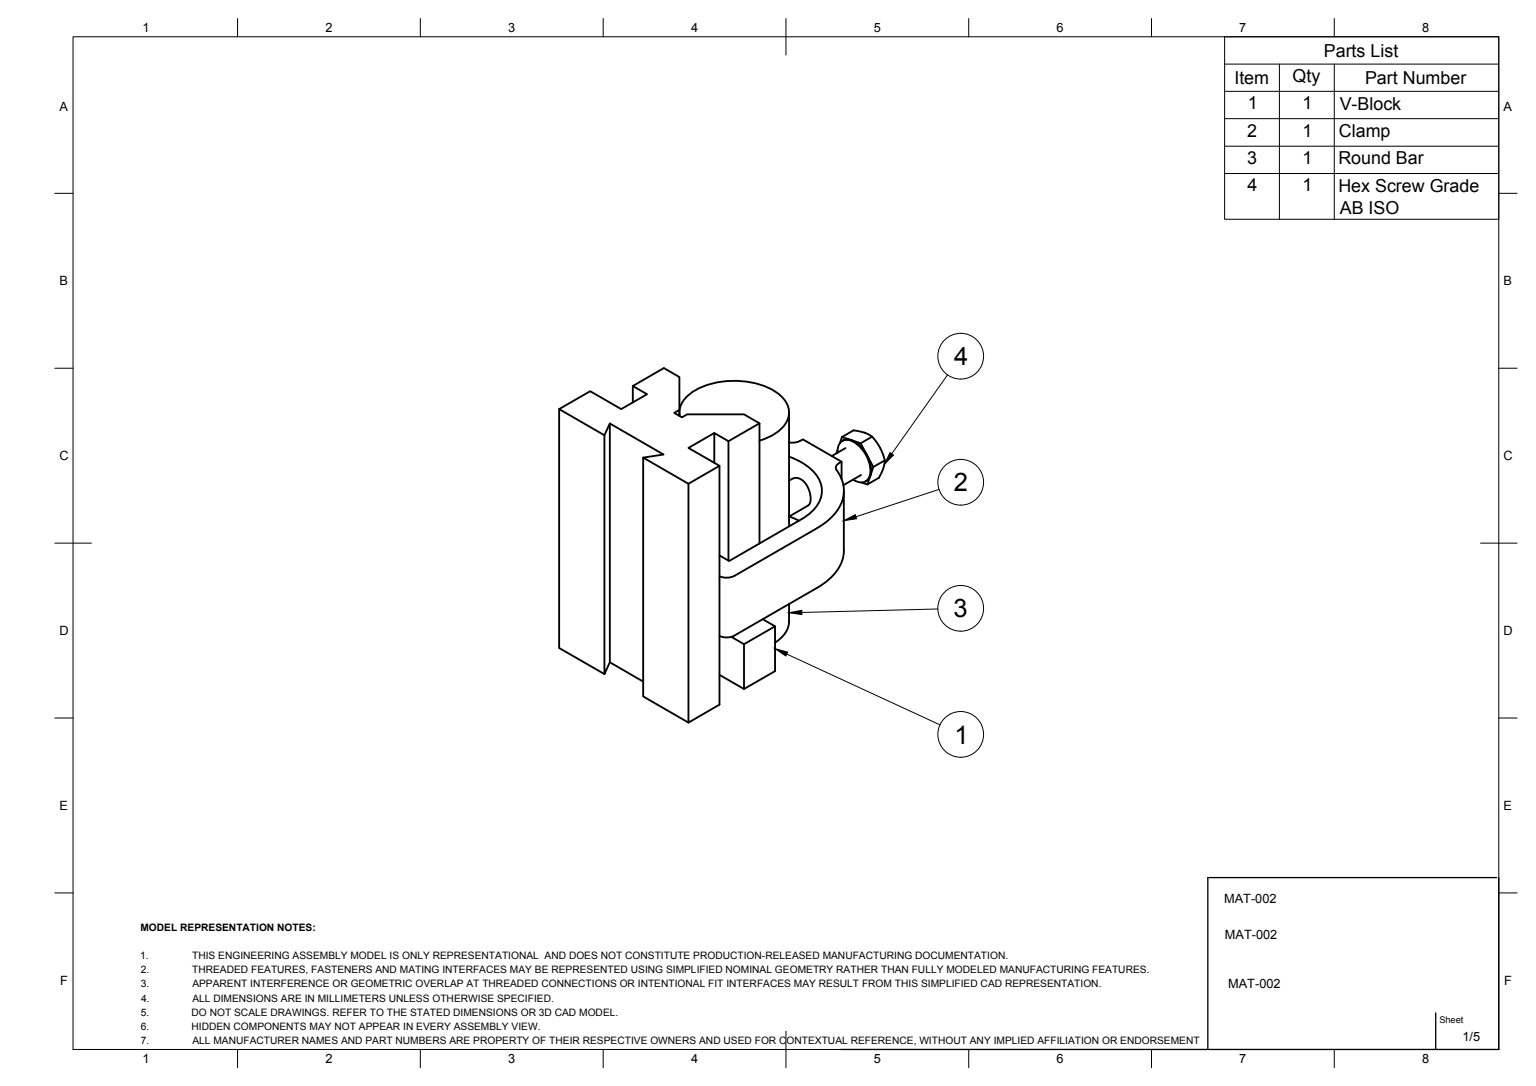
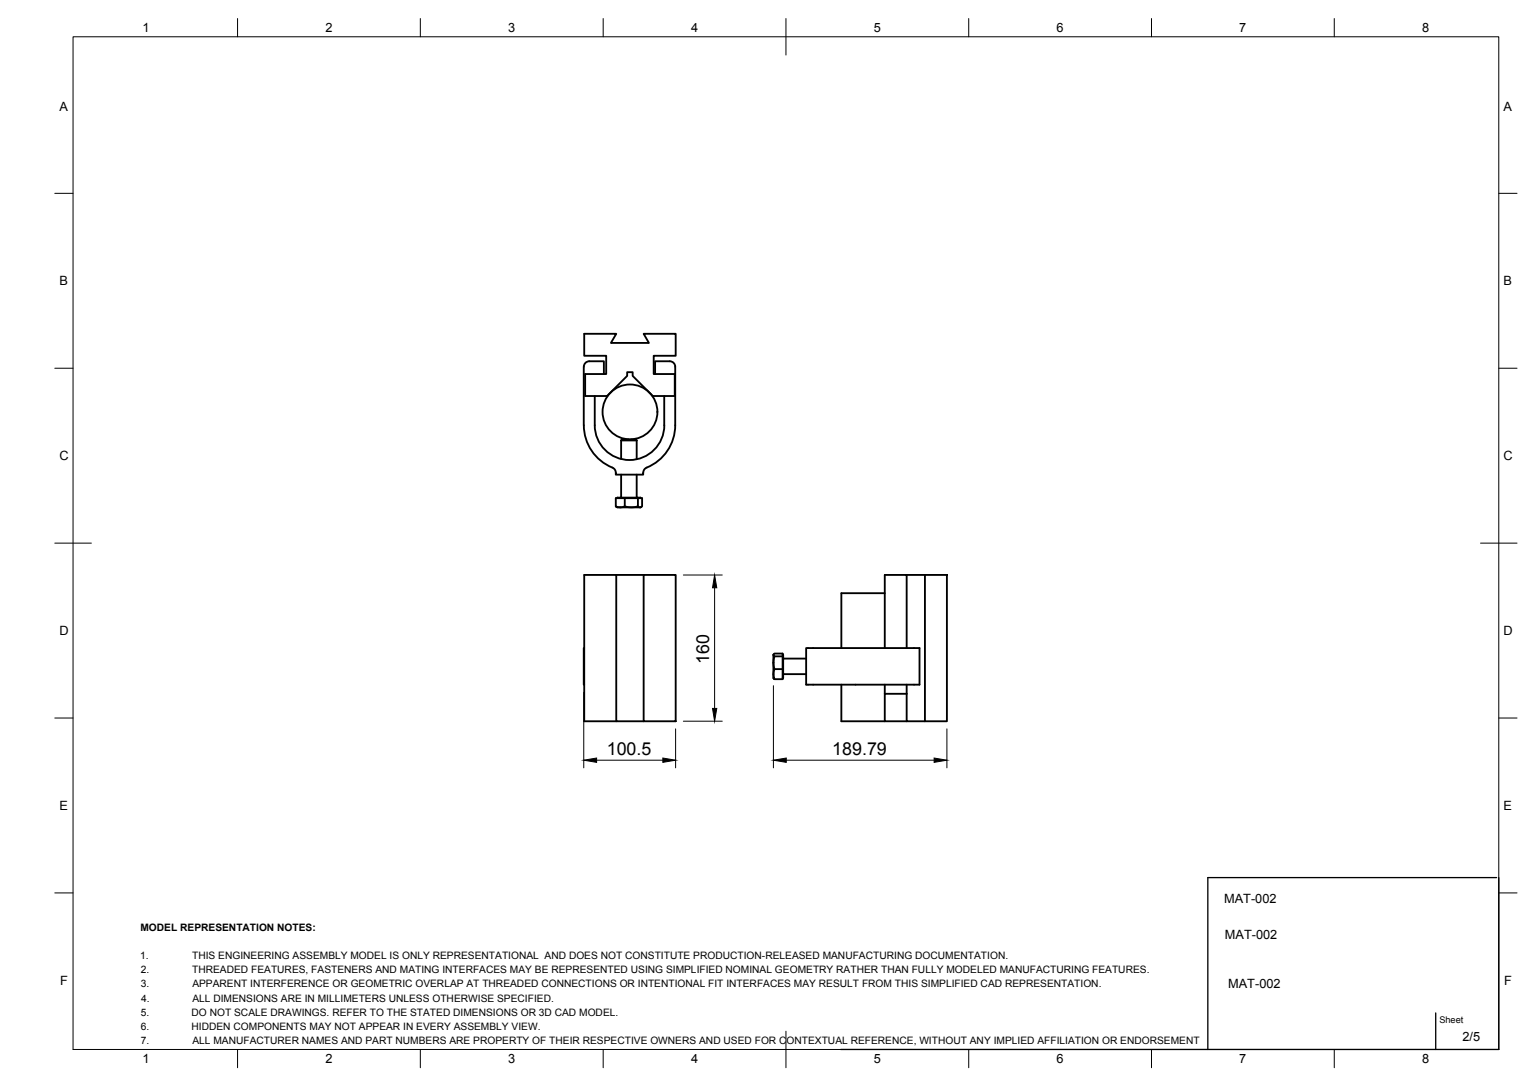
ISO-10303-21;
HEADER;
/* Generated by software containing ST-Developer
 * from STEP Tools, Inc. (www.steptools.com) 
 */

FILE_DESCRIPTION(
/* description */ ('STEP AP214'),
/* implementation_level */ '2;1');

FILE_NAME(
/* name */ 'MAT-002.step',
/* time_stamp */ '2026-11-14T04:35:10-08:00',
/* author */ (''),
/* organization */ (''),
/* preprocessor_version */ 'ST-DEVELOPER v20.2',
/* originating_system */ 'Autodesk Translation Framework v15.17.0.0',
/* authorisation */ '');

FILE_SCHEMA (('AUTOMOTIVE_DESIGN { 1 0 10303 214 3 1 1 }'));
ENDSEC;

DATA;
#10=MECHANICAL_DESIGN_GEOMETRIC_PRESENTATION_REPRESENTATION('',(#107,#108,
#109,#110),#2477);
#11=ITEM_DEFINED_TRANSFORMATION($,$,#1477,#1596);
#12=ITEM_DEFINED_TRANSFORMATION($,$,#1506,#1597);
#13=ITEM_DEFINED_TRANSFORMATION($,$,#1545,#1598);
#14=ITEM_DEFINED_TRANSFORMATION($,$,#1551,#1599);
#15=(
REPRESENTATION_RELATIONSHIP($,$,#2497,#2496)
REPRESENTATION_RELATIONSHIP_WITH_TRANSFORMATION(#11)
SHAPE_REPRESENTATION_RELATIONSHIP()
);
#16=(
REPRESENTATION_RELATIONSHIP($,$,#2498,#2496)
REPRESENTATION_RELATIONSHIP_WITH_TRANSFORMATION(#12)
SHAPE_REPRESENTATION_RELATIONSHIP()
);
#17=(
REPRESENTATION_RELATIONSHIP($,$,#2499,#2496)
REPRESENTATION_RELATIONSHIP_WITH_TRANSFORMATION(#13)
SHAPE_REPRESENTATION_RELATIONSHIP()
);
#18=(
REPRESENTATION_RELATIONSHIP($,$,#2500,#2496)
REPRESENTATION_RELATIONSHIP_WITH_TRANSFORMATION(#14)
SHAPE_REPRESENTATION_RELATIONSHIP()
);
#19=CONTEXT_DEPENDENT_SHAPE_REPRESENTATION(#15,#2492);
#20=CONTEXT_DEPENDENT_SHAPE_REPRESENTATION(#16,#2493);
#21=CONTEXT_DEPENDENT_SHAPE_REPRESENTATION(#17,#2494);
#22=CONTEXT_DEPENDENT_SHAPE_REPRESENTATION(#18,#2495);
#23=NEXT_ASSEMBLY_USAGE_OCCURRENCE('V-Block:1','V-Block:1','V-Block:1',
#2502,#2503,'V-Block:1');
#24=NEXT_ASSEMBLY_USAGE_OCCURRENCE('Clamp:1','Clamp:1','Clamp:1',#2502,
#2504,'Clamp:1');
#25=NEXT_ASSEMBLY_USAGE_OCCURRENCE('Round Bar:1','Round Bar:1',
'Round Bar:1',#2502,#2505,'Round Bar:1');
#26=NEXT_ASSEMBLY_USAGE_OCCURRENCE('Hex Screw Grade AB ISO:1',
'Hex Screw Grade AB ISO:1','Hex Screw Grade AB ISO:1',#2502,#2506,
'Hex Screw Grade AB ISO:1');
#27=(
BOUNDED_CURVE()
B_SPLINE_CURVE(2,(#2404,#2405,#2406),.UNSPECIFIED.,.F.,.F.)
B_SPLINE_CURVE_WITH_KNOTS((3,3),(-3.12660138416105,-1.84743207297635),
 .UNSPECIFIED.)
CURVE()
GEOMETRIC_REPRESENTATION_ITEM()
RATIONAL_B_SPLINE_CURVE((1.7511213796222,1.7511213796222,1.62539652116965))
REPRESENTATION_ITEM('')
);
#28=(
BOUNDED_CURVE()
B_SPLINE_CURVE(2,(#2407,#2408,#2409),.UNSPECIFIED.,.F.,.F.)
B_SPLINE_CURVE_WITH_KNOTS((3,3),(-4.40577069534575,-3.12660138416105),
 .UNSPECIFIED.)
CURVE()
GEOMETRIC_REPRESENTATION_ITEM()
RATIONAL_B_SPLINE_CURVE((1.62539652116964,1.75112137962219,1.75112137962219))
REPRESENTATION_ITEM('')
);
#29=(
BOUNDED_CURVE()
B_SPLINE_CURVE(2,(#2412,#2413,#2414),.UNSPECIFIED.,.F.,.F.)
B_SPLINE_CURVE_WITH_KNOTS((3,3),(-3.12660138416105,-1.84743207297636),
 .UNSPECIFIED.)
CURVE()
GEOMETRIC_REPRESENTATION_ITEM()
RATIONAL_B_SPLINE_CURVE((1.75112137962219,1.75112137962219,1.62539652116965))
REPRESENTATION_ITEM('')
);
#30=(
BOUNDED_CURVE()
B_SPLINE_CURVE(2,(#2415,#2416,#2417),.UNSPECIFIED.,.F.,.F.)
B_SPLINE_CURVE_WITH_KNOTS((3,3),(-4.40577069534575,-3.12660138416105),
 .UNSPECIFIED.)
CURVE()
GEOMETRIC_REPRESENTATION_ITEM()
RATIONAL_B_SPLINE_CURVE((1.62539652116965,1.7511213796222,1.7511213796222))
REPRESENTATION_ITEM('')
);
#31=(
BOUNDED_CURVE()
B_SPLINE_CURVE(2,(#2420,#2421,#2422),.UNSPECIFIED.,.F.,.F.)
B_SPLINE_CURVE_WITH_KNOTS((3,3),(-4.40577069534574,-3.12660138416105),
 .UNSPECIFIED.)
CURVE()
GEOMETRIC_REPRESENTATION_ITEM()
RATIONAL_B_SPLINE_CURVE((1.62539652116965,1.7511213796222,1.7511213796222))
REPRESENTATION_ITEM('')
);
#32=(
BOUNDED_CURVE()
B_SPLINE_CURVE(2,(#2423,#2424,#2425),.UNSPECIFIED.,.F.,.F.)
B_SPLINE_CURVE_WITH_KNOTS((3,3),(-3.12660138416105,-1.84743207297636),
 .UNSPECIFIED.)
CURVE()
GEOMETRIC_REPRESENTATION_ITEM()
RATIONAL_B_SPLINE_CURVE((1.75112137962219,1.75112137962219,1.62539652116965))
REPRESENTATION_ITEM('')
);
#33=(
BOUNDED_CURVE()
B_SPLINE_CURVE(2,(#2428,#2429,#2430),.UNSPECIFIED.,.F.,.F.)
B_SPLINE_CURVE_WITH_KNOTS((3,3),(-4.40577069534576,-3.12660138416105),
 .UNSPECIFIED.)
CURVE()
GEOMETRIC_REPRESENTATION_ITEM()
RATIONAL_B_SPLINE_CURVE((1.62539652116965,1.7511213796222,1.7511213796222))
REPRESENTATION_ITEM('')
);
#34=(
BOUNDED_CURVE()
B_SPLINE_CURVE(2,(#2431,#2432,#2433),.UNSPECIFIED.,.F.,.F.)
B_SPLINE_CURVE_WITH_KNOTS((3,3),(-3.12660138416105,-1.84743207297636),
 .UNSPECIFIED.)
CURVE()
GEOMETRIC_REPRESENTATION_ITEM()
RATIONAL_B_SPLINE_CURVE((1.75112137962219,1.75112137962219,1.62539652116965))
REPRESENTATION_ITEM('')
);
#35=(
BOUNDED_CURVE()
B_SPLINE_CURVE(2,(#2436,#2437,#2438),.UNSPECIFIED.,.F.,.F.)
B_SPLINE_CURVE_WITH_KNOTS((3,3),(-3.12660138416105,-1.84743207297636),
 .UNSPECIFIED.)
CURVE()
GEOMETRIC_REPRESENTATION_ITEM()
RATIONAL_B_SPLINE_CURVE((1.75112137962219,1.75112137962219,1.62539652116965))
REPRESENTATION_ITEM('')
);
#36=(
BOUNDED_CURVE()
B_SPLINE_CURVE(2,(#2439,#2440,#2441),.UNSPECIFIED.,.F.,.F.)
B_SPLINE_CURVE_WITH_KNOTS((3,3),(-4.40577069534574,-3.12660138416105),
 .UNSPECIFIED.)
CURVE()
GEOMETRIC_REPRESENTATION_ITEM()
RATIONAL_B_SPLINE_CURVE((1.62539652116965,1.75112137962219,1.75112137962219))
REPRESENTATION_ITEM('')
);
#37=(
BOUNDED_CURVE()
B_SPLINE_CURVE(2,(#2444,#2445,#2446),.UNSPECIFIED.,.F.,.F.)
B_SPLINE_CURVE_WITH_KNOTS((3,3),(-4.40577069534575,-3.12660138416105),
 .UNSPECIFIED.)
CURVE()
GEOMETRIC_REPRESENTATION_ITEM()
RATIONAL_B_SPLINE_CURVE((1.62539652116965,1.75112137962219,1.75112137962219))
REPRESENTATION_ITEM('')
);
#38=(
BOUNDED_CURVE()
B_SPLINE_CURVE(2,(#2447,#2448,#2449),.UNSPECIFIED.,.F.,.F.)
B_SPLINE_CURVE_WITH_KNOTS((3,3),(-3.12660138416105,-1.84743207297636),
 .UNSPECIFIED.)
CURVE()
GEOMETRIC_REPRESENTATION_ITEM()
RATIONAL_B_SPLINE_CURVE((1.75112137962219,1.75112137962219,1.62539652116964))
REPRESENTATION_ITEM('')
);
#39=CONICAL_SURFACE('',#1565,7.33266666666667,0.785398163397449);
#40=CONICAL_SURFACE('',#1584,12.75,1.0471975511966);
#41=CONICAL_SURFACE('',#1585,12.75,1.0471975511966);
#42=CONICAL_SURFACE('',#1586,12.75,1.0471975511966);
#43=CONICAL_SURFACE('',#1587,12.75,1.0471975511966);
#44=CONICAL_SURFACE('',#1588,12.75,1.0471975511966);
#45=CONICAL_SURFACE('',#1589,12.75,1.0471975511966);
#46=TOROIDAL_SURFACE('',#1552,9.06666666666667,0.566666666666667);
#47=FACE_BOUND('',#226,.T.);
#48=FACE_BOUND('',#235,.T.);
#49=FACE_BOUND('',#255,.T.);
#50=CIRCLE('',#1508,8.49999999999998);
#51=CIRCLE('',#1512,38.);
#52=CIRCLE('',#1513,38.);
#53=CIRCLE('',#1520,50.);
#54=CIRCLE('',#1521,50.);
#55=CIRCLE('',#1526,50.);
#56=CIRCLE('',#1527,50.);
#57=CIRCLE('',#1532,6.);
#58=CIRCLE('',#1533,6.);
#59=CIRCLE('',#1534,6.);
#60=CIRCLE('',#1535,6.);
#61=CIRCLE('',#1537,6.);
#62=CIRCLE('',#1538,6.);
#63=CIRCLE('',#1539,6.);
#64=CIRCLE('',#1540,6.);
#65=CIRCLE('',#1547,30.);
#66=CIRCLE('',#1548,30.);
#67=CIRCLE('',#1553,8.5);
#68=CIRCLE('',#1554,8.5);
#69=CIRCLE('',#1555,0.566666666666667);
#70=CIRCLE('',#1556,9.06666666666667);
#71=CIRCLE('',#1558,12.75);
#72=CIRCLE('',#1559,12.75);
#73=CIRCLE('',#1560,12.75);
#74=CIRCLE('',#1561,12.75);
#75=CIRCLE('',#1562,12.75);
#76=CIRCLE('',#1563,12.75);
#77=CIRCLE('',#1564,12.75);
#78=CIRCLE('',#1566,8.5);
#79=CIRCLE('',#1567,7.33266666666667);
#80=CIRCLE('',#1578,12.75);
#81=CIRCLE('',#1579,12.75);
#82=CIRCLE('',#1580,12.75);
#83=CIRCLE('',#1581,12.75);
#84=CIRCLE('',#1582,12.75);
#85=CIRCLE('',#1583,12.75);
#86=B_SPLINE_CURVE_WITH_KNOTS('',3,(#2159,#2160,#2161,#2162,#2163,#2164,
#2165,#2166,#2167,#2168,#2169,#2170,#2171,#2172,#2173,#2174,#2175,#2176,
#2177),.UNSPECIFIED.,.F.,.F.,(4,2,2,2,3,2,2,2,4),(3.85552474626411,4.17737028900463,
4.49921583174514,4.82064221776852,5.14206860379189,5.46349498981527,5.78492137583865,
6.10676691857916,6.42861246131968),.UNSPECIFIED.);
#87=B_SPLINE_CURVE_WITH_KNOTS('',3,(#2181,#2182,#2183,#2184,#2185,#2186,
#2187,#2188,#2189,#2190,#2191,#2192,#2193,#2194,#2195,#2196,#2197,#2198),
 .UNSPECIFIED.,.F.,.F.,(4,2,2,2,2,2,2,2,4),(6.42861246131968,6.74954370836776,
7.07047495541584,7.39178893055184,7.71310290568784,8.03441688082384,8.35573085595985,
8.67666210300793,8.99759335005601),.UNSPECIFIED.);
#88=CYLINDRICAL_SURFACE('',#1507,8.49999999999998);
#89=CYLINDRICAL_SURFACE('',#1511,38.);
#90=CYLINDRICAL_SURFACE('',#1519,50.);
#91=CYLINDRICAL_SURFACE('',#1525,50.);
#92=CYLINDRICAL_SURFACE('',#1541,6.);
#93=CYLINDRICAL_SURFACE('',#1542,6.);
#94=CYLINDRICAL_SURFACE('',#1543,6.);
#95=CYLINDRICAL_SURFACE('',#1544,6.);
#96=CYLINDRICAL_SURFACE('',#1546,30.);
#97=CYLINDRICAL_SURFACE('',#1557,12.75);
#98=CYLINDRICAL_SURFACE('',#1568,8.5);
#99=SHAPE_REPRESENTATION_RELATIONSHIP('SRR','None',#2497,#103);
#100=SHAPE_REPRESENTATION_RELATIONSHIP('SRR','None',#2498,#104);
#101=SHAPE_REPRESENTATION_RELATIONSHIP('SRR','None',#2499,#105);
#102=SHAPE_REPRESENTATION_RELATIONSHIP('SRR','None',#2500,#106);
#103=ADVANCED_BREP_SHAPE_REPRESENTATION('',(#111),#2473);
#104=ADVANCED_BREP_SHAPE_REPRESENTATION('',(#112),#2474);
#105=ADVANCED_BREP_SHAPE_REPRESENTATION('',(#113),#2475);
#106=ADVANCED_BREP_SHAPE_REPRESENTATION('',(#114),#2476);
#107=STYLED_ITEM('',(#2526),#111);
#108=STYLED_ITEM('',(#2527),#112);
#109=STYLED_ITEM('',(#2528),#113);
#110=STYLED_ITEM('',(#2529),#114);
#111=MANIFOLD_SOLID_BREP('Body1',#1427);
#112=MANIFOLD_SOLID_BREP('Body1',#1428);
#113=MANIFOLD_SOLID_BREP('Body1',#1429);
#114=MANIFOLD_SOLID_BREP('Body1',#1430);
#115=FACE_OUTER_BOUND('',#194,.T.);
#116=FACE_OUTER_BOUND('',#195,.T.);
#117=FACE_OUTER_BOUND('',#196,.T.);
#118=FACE_OUTER_BOUND('',#197,.T.);
#119=FACE_OUTER_BOUND('',#198,.T.);
#120=FACE_OUTER_BOUND('',#199,.T.);
#121=FACE_OUTER_BOUND('',#200,.T.);
#122=FACE_OUTER_BOUND('',#201,.T.);
#123=FACE_OUTER_BOUND('',#202,.T.);
#124=FACE_OUTER_BOUND('',#203,.T.);
#125=FACE_OUTER_BOUND('',#204,.T.);
#126=FACE_OUTER_BOUND('',#205,.T.);
#127=FACE_OUTER_BOUND('',#206,.T.);
#128=FACE_OUTER_BOUND('',#207,.T.);
#129=FACE_OUTER_BOUND('',#208,.T.);
#130=FACE_OUTER_BOUND('',#209,.T.);
#131=FACE_OUTER_BOUND('',#210,.T.);
#132=FACE_OUTER_BOUND('',#211,.T.);
#133=FACE_OUTER_BOUND('',#212,.T.);
#134=FACE_OUTER_BOUND('',#213,.T.);
#135=FACE_OUTER_BOUND('',#214,.T.);
#136=FACE_OUTER_BOUND('',#215,.T.);
#137=FACE_OUTER_BOUND('',#216,.T.);
#138=FACE_OUTER_BOUND('',#217,.T.);
#139=FACE_OUTER_BOUND('',#218,.T.);
#140=FACE_OUTER_BOUND('',#219,.T.);
#141=FACE_OUTER_BOUND('',#220,.T.);
#142=FACE_OUTER_BOUND('',#221,.T.);
#143=FACE_OUTER_BOUND('',#222,.T.);
#144=FACE_OUTER_BOUND('',#223,.T.);
#145=FACE_OUTER_BOUND('',#224,.T.);
#146=FACE_OUTER_BOUND('',#225,.T.);
#147=FACE_OUTER_BOUND('',#227,.T.);
#148=FACE_OUTER_BOUND('',#228,.T.);
#149=FACE_OUTER_BOUND('',#229,.T.);
#150=FACE_OUTER_BOUND('',#230,.T.);
#151=FACE_OUTER_BOUND('',#231,.T.);
#152=FACE_OUTER_BOUND('',#232,.T.);
#153=FACE_OUTER_BOUND('',#233,.T.);
#154=FACE_OUTER_BOUND('',#234,.T.);
#155=FACE_OUTER_BOUND('',#236,.T.);
#156=FACE_OUTER_BOUND('',#237,.T.);
#157=FACE_OUTER_BOUND('',#238,.T.);
#158=FACE_OUTER_BOUND('',#239,.T.);
#159=FACE_OUTER_BOUND('',#240,.T.);
#160=FACE_OUTER_BOUND('',#241,.T.);
#161=FACE_OUTER_BOUND('',#242,.T.);
#162=FACE_OUTER_BOUND('',#243,.T.);
#163=FACE_OUTER_BOUND('',#244,.T.);
#164=FACE_OUTER_BOUND('',#245,.T.);
#165=FACE_OUTER_BOUND('',#246,.T.);
#166=FACE_OUTER_BOUND('',#247,.T.);
#167=FACE_OUTER_BOUND('',#248,.T.);
#168=FACE_OUTER_BOUND('',#249,.T.);
#169=FACE_OUTER_BOUND('',#250,.T.);
#170=FACE_OUTER_BOUND('',#251,.T.);
#171=FACE_OUTER_BOUND('',#252,.T.);
#172=FACE_OUTER_BOUND('',#253,.T.);
#173=FACE_OUTER_BOUND('',#254,.T.);
#174=FACE_OUTER_BOUND('',#256,.T.);
#175=FACE_OUTER_BOUND('',#257,.T.);
#176=FACE_OUTER_BOUND('',#258,.T.);
#177=FACE_OUTER_BOUND('',#259,.T.);
#178=FACE_OUTER_BOUND('',#260,.T.);
#179=FACE_OUTER_BOUND('',#261,.T.);
#180=FACE_OUTER_BOUND('',#262,.T.);
#181=FACE_OUTER_BOUND('',#263,.T.);
#182=FACE_OUTER_BOUND('',#264,.T.);
#183=FACE_OUTER_BOUND('',#265,.T.);
#184=FACE_OUTER_BOUND('',#266,.T.);
#185=FACE_OUTER_BOUND('',#267,.T.);
#186=FACE_OUTER_BOUND('',#268,.T.);
#187=FACE_OUTER_BOUND('',#269,.T.);
#188=FACE_OUTER_BOUND('',#270,.T.);
#189=FACE_OUTER_BOUND('',#271,.T.);
#190=FACE_OUTER_BOUND('',#272,.T.);
#191=FACE_OUTER_BOUND('',#273,.T.);
#192=FACE_OUTER_BOUND('',#274,.T.);
#193=FACE_OUTER_BOUND('',#275,.T.);
#194=EDGE_LOOP('',(#894,#895,#896,#897));
#195=EDGE_LOOP('',(#898,#899,#900,#901));
#196=EDGE_LOOP('',(#902,#903,#904,#905));
#197=EDGE_LOOP('',(#906,#907,#908,#909));
#198=EDGE_LOOP('',(#910,#911,#912,#913));
#199=EDGE_LOOP('',(#914,#915,#916,#917,#918,#919));
#200=EDGE_LOOP('',(#920,#921,#922,#923,#924,#925));
#201=EDGE_LOOP('',(#926,#927,#928,#929));
#202=EDGE_LOOP('',(#930,#931,#932,#933));
#203=EDGE_LOOP('',(#934,#935,#936,#937));
#204=EDGE_LOOP('',(#938,#939,#940,#941));
#205=EDGE_LOOP('',(#942,#943,#944,#945));
#206=EDGE_LOOP('',(#946,#947,#948,#949,#950,#951));
#207=EDGE_LOOP('',(#952,#953,#954,#955,#956,#957));
#208=EDGE_LOOP('',(#958,#959,#960,#961));
#209=EDGE_LOOP('',(#962,#963,#964,#965));
#210=EDGE_LOOP('',(#966,#967,#968,#969));
#211=EDGE_LOOP('',(#970,#971,#972,#973));
#212=EDGE_LOOP('',(#974,#975,#976,#977));
#213=EDGE_LOOP('',(#978,#979,#980,#981));
#214=EDGE_LOOP('',(#982,#983,#984,#985));
#215=EDGE_LOOP('',(#986,#987,#988,#989));
#216=EDGE_LOOP('',(#990,#991,#992,#993,#994,#995,#996,#997,#998,#999,#1000,
#1001,#1002,#1003,#1004,#1005,#1006,#1007,#1008,#1009,#1010,#1011));
#217=EDGE_LOOP('',(#1012,#1013,#1014,#1015,#1016,#1017,#1018,#1019,#1020,
#1021,#1022,#1023,#1024,#1025,#1026,#1027,#1028,#1029,#1030,#1031,#1032,
#1033));
#218=EDGE_LOOP('',(#1034,#1035,#1036,#1037));
#219=EDGE_LOOP('',(#1038,#1039,#1040,#1041));
#220=EDGE_LOOP('',(#1042,#1043,#1044,#1045));
#221=EDGE_LOOP('',(#1046,#1047,#1048,#1049));
#222=EDGE_LOOP('',(#1050,#1051,#1052,#1053,#1054));
#223=EDGE_LOOP('',(#1055,#1056,#1057,#1058));
#224=EDGE_LOOP('',(#1059,#1060,#1061,#1062));
#225=EDGE_LOOP('',(#1063,#1064,#1065,#1066));
#226=EDGE_LOOP('',(#1067,#1068));
#227=EDGE_LOOP('',(#1069,#1070,#1071,#1072));
#228=EDGE_LOOP('',(#1073,#1074,#1075,#1076));
#229=EDGE_LOOP('',(#1077,#1078,#1079,#1080));
#230=EDGE_LOOP('',(#1081,#1082,#1083,#1084));
#231=EDGE_LOOP('',(#1085,#1086,#1087,#1088));
#232=EDGE_LOOP('',(#1089,#1090,#1091,#1092));
#233=EDGE_LOOP('',(#1093,#1094,#1095,#1096));
#234=EDGE_LOOP('',(#1097,#1098,#1099,#1100));
#235=EDGE_LOOP('',(#1101));
#236=EDGE_LOOP('',(#1102,#1103,#1104,#1105));
#237=EDGE_LOOP('',(#1106,#1107,#1108,#1109));
#238=EDGE_LOOP('',(#1110,#1111,#1112,#1113));
#239=EDGE_LOOP('',(#1114,#1115,#1116,#1117));
#240=EDGE_LOOP('',(#1118,#1119,#1120,#1121));
#241=EDGE_LOOP('',(#1122,#1123,#1124,#1125,#1126,#1127,#1128,#1129,#1130,
#1131,#1132,#1133,#1134,#1135,#1136,#1137,#1138,#1139,#1140,#1141));
#242=EDGE_LOOP('',(#1142,#1143,#1144,#1145,#1146,#1147,#1148,#1149,#1150,
#1151,#1152,#1153,#1154,#1155,#1156,#1157,#1158,#1159,#1160,#1161));
#243=EDGE_LOOP('',(#1162,#1163,#1164,#1165));
#244=EDGE_LOOP('',(#1166,#1167,#1168,#1169));
#245=EDGE_LOOP('',(#1170,#1171,#1172,#1173));
#246=EDGE_LOOP('',(#1174,#1175,#1176,#1177));
#247=EDGE_LOOP('',(#1178,#1179,#1180,#1181));
#248=EDGE_LOOP('',(#1182));
#249=EDGE_LOOP('',(#1183));
#250=EDGE_LOOP('',(#1184,#1185,#1186,#1187,#1188));
#251=EDGE_LOOP('',(#1189,#1190,#1191,#1192,#1193,#1194,#1195,#1196,#1197));
#252=EDGE_LOOP('',(#1198,#1199,#1200,#1201));
#253=EDGE_LOOP('',(#1202,#1203,#1204,#1205,#1206));
#254=EDGE_LOOP('',(#1207));
#255=EDGE_LOOP('',(#1208));
#256=EDGE_LOOP('',(#1209));
#257=EDGE_LOOP('',(#1210,#1211,#1212));
#258=EDGE_LOOP('',(#1213,#1214,#1215));
#259=EDGE_LOOP('',(#1216,#1217,#1218));
#260=EDGE_LOOP('',(#1219,#1220,#1221));
#261=EDGE_LOOP('',(#1222,#1223,#1224));
#262=EDGE_LOOP('',(#1225,#1226,#1227));
#263=EDGE_LOOP('',(#1228,#1229,#1230,#1231,#1232,#1233));
#264=EDGE_LOOP('',(#1234,#1235,#1236));
#265=EDGE_LOOP('',(#1237,#1238,#1239));
#266=EDGE_LOOP('',(#1240,#1241,#1242));
#267=EDGE_LOOP('',(#1243,#1244,#1245));
#268=EDGE_LOOP('',(#1246,#1247,#1248));
#269=EDGE_LOOP('',(#1249,#1250,#1251));
#270=EDGE_LOOP('',(#1252,#1253,#1254,#1255,#1256,#1257));
#271=EDGE_LOOP('',(#1258,#1259,#1260,#1261,#1262,#1263));
#272=EDGE_LOOP('',(#1264,#1265,#1266,#1267,#1268,#1269));
#273=EDGE_LOOP('',(#1270,#1271,#1272,#1273,#1274,#1275));
#274=EDGE_LOOP('',(#1276,#1277,#1278,#1279,#1280,#1281));
#275=EDGE_LOOP('',(#1282,#1283,#1284,#1285,#1286,#1287));
#276=LINE('',#2000,#423);
#277=LINE('',#2002,#424);
#278=LINE('',#2004,#425);
#279=LINE('',#2005,#426);
#280=LINE('',#2009,#427);
#281=LINE('',#2011,#428);
#282=LINE('',#2013,#429);
#283=LINE('',#2014,#430);
#284=LINE('',#2018,#431);
#285=LINE('',#2020,#432);
#286=LINE('',#2022,#433);
#287=LINE('',#2023,#434);
#288=LINE('',#2026,#435);
#289=LINE('',#2028,#436);
#290=LINE('',#2029,#437);
#291=LINE('',#2032,#438);
#292=LINE('',#2034,#439);
#293=LINE('',#2035,#440);
#294=LINE('',#2037,#441);
#295=LINE('',#2039,#442);
#296=LINE('',#2041,#443);
#297=LINE('',#2042,#444);
#298=LINE('',#2045,#445);
#299=LINE('',#2047,#446);
#300=LINE('',#2049,#447);
#301=LINE('',#2051,#448);
#302=LINE('',#2052,#449);
#303=LINE('',#2055,#450);
#304=LINE('',#2057,#451);
#305=LINE('',#2058,#452);
#306=LINE('',#2061,#453);
#307=LINE('',#2063,#454);
#308=LINE('',#2064,#455);
#309=LINE('',#2067,#456);
#310=LINE('',#2069,#457);
#311=LINE('',#2070,#458);
#312=LINE('',#2073,#459);
#313=LINE('',#2075,#460);
#314=LINE('',#2076,#461);
#315=LINE('',#2079,#462);
#316=LINE('',#2081,#463);
#317=LINE('',#2082,#464);
#318=LINE('',#2084,#465);
#319=LINE('',#2086,#466);
#320=LINE('',#2088,#467);
#321=LINE('',#2089,#468);
#322=LINE('',#2092,#469);
#323=LINE('',#2094,#470);
#324=LINE('',#2096,#471);
#325=LINE('',#2098,#472);
#326=LINE('',#2099,#473);
#327=LINE('',#2102,#474);
#328=LINE('',#2104,#475);
#329=LINE('',#2105,#476);
#330=LINE('',#2108,#477);
#331=LINE('',#2110,#478);
#332=LINE('',#2111,#479);
#333=LINE('',#2114,#480);
#334=LINE('',#2116,#481);
#335=LINE('',#2117,#482);
#336=LINE('',#2120,#483);
#337=LINE('',#2122,#484);
#338=LINE('',#2123,#485);
#339=LINE('',#2126,#486);
#340=LINE('',#2128,#487);
#341=LINE('',#2129,#488);
#342=LINE('',#2132,#489);
#343=LINE('',#2134,#490);
#344=LINE('',#2135,#491);
#345=LINE('',#2138,#492);
#346=LINE('',#2140,#493);
#347=LINE('',#2141,#494);
#348=LINE('',#2143,#495);
#349=LINE('',#2144,#496);
#350=LINE('',#2146,#497);
#351=LINE('',#2147,#498);
#352=LINE('',#2150,#499);
#353=LINE('',#2153,#500);
#354=LINE('',#2179,#501);
#355=LINE('',#2202,#502);
#356=LINE('',#2204,#503);
#357=LINE('',#2206,#504);
#358=LINE('',#2207,#505);
#359=LINE('',#2210,#506);
#360=LINE('',#2212,#507);
#361=LINE('',#2213,#508);
#362=LINE('',#2218,#509);
#363=LINE('',#2222,#510);
#364=LINE('',#2224,#511);
#365=LINE('',#2225,#512);
#366=LINE('',#2228,#513);
#367=LINE('',#2230,#514);
#368=LINE('',#2231,#515);
#369=LINE('',#2234,#516);
#370=LINE('',#2236,#517);
#371=LINE('',#2237,#518);
#372=LINE('',#2240,#519);
#373=LINE('',#2242,#520);
#374=LINE('',#2243,#521);
#375=LINE('',#2247,#522);
#376=LINE('',#2249,#523);
#377=LINE('',#2251,#524);
#378=LINE('',#2252,#525);
#379=LINE('',#2257,#526);
#380=LINE('',#2262,#527);
#381=LINE('',#2264,#528);
#382=LINE('',#2266,#529);
#383=LINE('',#2267,#530);
#384=LINE('',#2270,#531);
#385=LINE('',#2272,#532);
#386=LINE('',#2273,#533);
#387=LINE('',#2276,#534);
#388=LINE('',#2278,#535);
#389=LINE('',#2279,#536);
#390=LINE('',#2285,#537);
#391=LINE('',#2288,#538);
#392=LINE('',#2291,#539);
#393=LINE('',#2293,#540);
#394=LINE('',#2294,#541);
#395=LINE('',#2298,#542);
#396=LINE('',#2300,#543);
#397=LINE('',#2302,#544);
#398=LINE('',#2303,#545);
#399=LINE('',#2305,#546);
#400=LINE('',#2306,#547);
#401=LINE('',#2326,#548);
#402=LINE('',#2348,#549);
#403=LINE('',#2359,#550);
#404=LINE('',#2362,#551);
#405=LINE('',#2367,#552);
#406=LINE('',#2368,#553);
#407=LINE('',#2371,#554);
#408=LINE('',#2372,#555);
#409=LINE('',#2375,#556);
#410=LINE('',#2376,#557);
#411=LINE('',#2379,#558);
#412=LINE('',#2380,#559);
#413=LINE('',#2383,#560);
#414=LINE('',#2384,#561);
#415=LINE('',#2387,#562);
#416=LINE('',#2388,#563);
#417=LINE('',#2451,#564);
#418=LINE('',#2452,#565);
#419=LINE('',#2454,#566);
#420=LINE('',#2456,#567);
#421=LINE('',#2458,#568);
#422=LINE('',#2460,#569);
#423=VECTOR('',#1606,1000.);
#424=VECTOR('',#1607,1000.);
#425=VECTOR('',#1608,1000.);
#426=VECTOR('',#1609,1000.);
#427=VECTOR('',#1612,1000.);
#428=VECTOR('',#1613,1000.);
#429=VECTOR('',#1614,1000.);
#430=VECTOR('',#1615,1000.);
#431=VECTOR('',#1618,1000.);
#432=VECTOR('',#1619,1000.);
#433=VECTOR('',#1620,1000.);
#434=VECTOR('',#1621,1000.);
#435=VECTOR('',#1624,1000.);
#436=VECTOR('',#1625,1000.);
#437=VECTOR('',#1626,1000.);
#438=VECTOR('',#1629,1000.);
#439=VECTOR('',#1630,1000.);
#440=VECTOR('',#1631,1000.);
#441=VECTOR('',#1634,1000.);
#442=VECTOR('',#1635,1000.);
#443=VECTOR('',#1636,1000.);
#444=VECTOR('',#1637,1000.);
#445=VECTOR('',#1640,1000.);
#446=VECTOR('',#1641,1000.);
#447=VECTOR('',#1642,1000.);
#448=VECTOR('',#1643,1000.);
#449=VECTOR('',#1644,1000.);
#450=VECTOR('',#1647,1000.);
#451=VECTOR('',#1648,1000.);
#452=VECTOR('',#1649,1000.);
#453=VECTOR('',#1652,1000.);
#454=VECTOR('',#1653,1000.);
#455=VECTOR('',#1654,1000.);
#456=VECTOR('',#1657,1000.);
#457=VECTOR('',#1658,1000.);
#458=VECTOR('',#1659,1000.);
#459=VECTOR('',#1662,1000.);
#460=VECTOR('',#1663,1000.);
#461=VECTOR('',#1664,1000.);
#462=VECTOR('',#1667,1000.);
#463=VECTOR('',#1668,1000.);
#464=VECTOR('',#1669,1000.);
#465=VECTOR('',#1672,1000.);
#466=VECTOR('',#1673,1000.);
#467=VECTOR('',#1674,1000.);
#468=VECTOR('',#1675,1000.);
#469=VECTOR('',#1678,1000.);
#470=VECTOR('',#1679,1000.);
#471=VECTOR('',#1680,1000.);
#472=VECTOR('',#1681,1000.);
#473=VECTOR('',#1682,1000.);
#474=VECTOR('',#1685,1000.);
#475=VECTOR('',#1686,1000.);
#476=VECTOR('',#1687,1000.);
#477=VECTOR('',#1690,1000.);
#478=VECTOR('',#1691,1000.);
#479=VECTOR('',#1692,1000.);
#480=VECTOR('',#1695,1000.);
#481=VECTOR('',#1696,1000.);
#482=VECTOR('',#1697,1000.);
#483=VECTOR('',#1700,1000.);
#484=VECTOR('',#1701,1000.);
#485=VECTOR('',#1702,1000.);
#486=VECTOR('',#1705,1000.);
#487=VECTOR('',#1706,1000.);
#488=VECTOR('',#1707,1000.);
#489=VECTOR('',#1710,1000.);
#490=VECTOR('',#1711,1000.);
#491=VECTOR('',#1712,1000.);
#492=VECTOR('',#1715,1000.);
#493=VECTOR('',#1716,1000.);
#494=VECTOR('',#1717,1000.);
#495=VECTOR('',#1720,1000.);
#496=VECTOR('',#1721,1000.);
#497=VECTOR('',#1724,1000.);
#498=VECTOR('',#1725,1000.);
#499=VECTOR('',#1730,1000.);
#500=VECTOR('',#1735,1000.);
#501=VECTOR('',#1742,8.49999999999998);
#502=VECTOR('',#1747,1000.);
#503=VECTOR('',#1748,1000.);
#504=VECTOR('',#1749,1000.);
#505=VECTOR('',#1750,1000.);
#506=VECTOR('',#1753,1000.);
#507=VECTOR('',#1754,1000.);
#508=VECTOR('',#1755,1000.);
#509=VECTOR('',#1760,1000.);
#510=VECTOR('',#1765,1000.);
#511=VECTOR('',#1766,1000.);
#512=VECTOR('',#1767,1000.);
#513=VECTOR('',#1770,1000.);
#514=VECTOR('',#1771,1000.);
#515=VECTOR('',#1772,1000.);
#516=VECTOR('',#1775,1000.);
#517=VECTOR('',#1776,1000.);
#518=VECTOR('',#1777,1000.);
#519=VECTOR('',#1780,1000.);
#520=VECTOR('',#1781,1000.);
#521=VECTOR('',#1782,1000.);
#522=VECTOR('',#1785,1000.);
#523=VECTOR('',#1786,1000.);
#524=VECTOR('',#1787,1000.);
#525=VECTOR('',#1788,1000.);
#526=VECTOR('',#1793,1000.);
#527=VECTOR('',#1798,1000.);
#528=VECTOR('',#1799,1000.);
#529=VECTOR('',#1800,1000.);
#530=VECTOR('',#1801,1000.);
#531=VECTOR('',#1804,1000.);
#532=VECTOR('',#1805,1000.);
#533=VECTOR('',#1806,1000.);
#534=VECTOR('',#1809,1000.);
#535=VECTOR('',#1810,1000.);
#536=VECTOR('',#1811,1000.);
#537=VECTOR('',#1816,1000.);
#538=VECTOR('',#1819,1000.);
#539=VECTOR('',#1822,1000.);
#540=VECTOR('',#1823,1000.);
#541=VECTOR('',#1824,1000.);
#542=VECTOR('',#1827,1000.);
#543=VECTOR('',#1828,1000.);
#544=VECTOR('',#1829,1000.);
#545=VECTOR('',#1830,1000.);
#546=VECTOR('',#1833,1000.);
#547=VECTOR('',#1834,1000.);
#548=VECTOR('',#1869,30.);
#549=VECTOR('',#1896,12.75);
#550=VECTOR('',#1909,7.33266666666667);
#551=VECTOR('',#1914,8.5);
#552=VECTOR('',#1921,1000.);
#553=VECTOR('',#1922,1000.);
#554=VECTOR('',#1925,1000.);
#555=VECTOR('',#1926,1000.);
#556=VECTOR('',#1929,1000.);
#557=VECTOR('',#1930,1000.);
#558=VECTOR('',#1933,1000.);
#559=VECTOR('',#1934,1000.);
#560=VECTOR('',#1937,1000.);
#561=VECTOR('',#1938,1000.);
#562=VECTOR('',#1941,1000.);
#563=VECTOR('',#1942,1000.);
#564=VECTOR('',#1971,1000.);
#565=VECTOR('',#1972,1000.);
#566=VECTOR('',#1975,1000.);
#567=VECTOR('',#1978,1000.);
#568=VECTOR('',#1981,1000.);
#569=VECTOR('',#1984,1000.);
#570=VERTEX_POINT('',#1998);
#571=VERTEX_POINT('',#1999);
#572=VERTEX_POINT('',#2001);
#573=VERTEX_POINT('',#2003);
#574=VERTEX_POINT('',#2007);
#575=VERTEX_POINT('',#2008);
#576=VERTEX_POINT('',#2010);
#577=VERTEX_POINT('',#2012);
#578=VERTEX_POINT('',#2016);
#579=VERTEX_POINT('',#2017);
#580=VERTEX_POINT('',#2019);
#581=VERTEX_POINT('',#2021);
#582=VERTEX_POINT('',#2025);
#583=VERTEX_POINT('',#2027);
#584=VERTEX_POINT('',#2031);
#585=VERTEX_POINT('',#2033);
#586=VERTEX_POINT('',#2038);
#587=VERTEX_POINT('',#2040);
#588=VERTEX_POINT('',#2044);
#589=VERTEX_POINT('',#2046);
#590=VERTEX_POINT('',#2048);
#591=VERTEX_POINT('',#2050);
#592=VERTEX_POINT('',#2054);
#593=VERTEX_POINT('',#2056);
#594=VERTEX_POINT('',#2060);
#595=VERTEX_POINT('',#2062);
#596=VERTEX_POINT('',#2066);
#597=VERTEX_POINT('',#2068);
#598=VERTEX_POINT('',#2072);
#599=VERTEX_POINT('',#2074);
#600=VERTEX_POINT('',#2078);
#601=VERTEX_POINT('',#2080);
#602=VERTEX_POINT('',#2085);
#603=VERTEX_POINT('',#2087);
#604=VERTEX_POINT('',#2091);
#605=VERTEX_POINT('',#2093);
#606=VERTEX_POINT('',#2095);
#607=VERTEX_POINT('',#2097);
#608=VERTEX_POINT('',#2101);
#609=VERTEX_POINT('',#2103);
#610=VERTEX_POINT('',#2107);
#611=VERTEX_POINT('',#2109);
#612=VERTEX_POINT('',#2113);
#613=VERTEX_POINT('',#2115);
#614=VERTEX_POINT('',#2119);
#615=VERTEX_POINT('',#2121);
#616=VERTEX_POINT('',#2125);
#617=VERTEX_POINT('',#2127);
#618=VERTEX_POINT('',#2131);
#619=VERTEX_POINT('',#2133);
#620=VERTEX_POINT('',#2137);
#621=VERTEX_POINT('',#2139);
#622=VERTEX_POINT('',#2157);
#623=VERTEX_POINT('',#2158);
#624=VERTEX_POINT('',#2178);
#625=VERTEX_POINT('',#2200);
#626=VERTEX_POINT('',#2201);
#627=VERTEX_POINT('',#2203);
#628=VERTEX_POINT('',#2205);
#629=VERTEX_POINT('',#2209);
#630=VERTEX_POINT('',#2211);
#631=VERTEX_POINT('',#2215);
#632=VERTEX_POINT('',#2217);
#633=VERTEX_POINT('',#2221);
#634=VERTEX_POINT('',#2223);
#635=VERTEX_POINT('',#2227);
#636=VERTEX_POINT('',#2229);
#637=VERTEX_POINT('',#2233);
#638=VERTEX_POINT('',#2235);
#639=VERTEX_POINT('',#2239);
#640=VERTEX_POINT('',#2241);
#641=VERTEX_POINT('',#2245);
#642=VERTEX_POINT('',#2246);
#643=VERTEX_POINT('',#2248);
#644=VERTEX_POINT('',#2250);
#645=VERTEX_POINT('',#2254);
#646=VERTEX_POINT('',#2256);
#647=VERTEX_POINT('',#2260);
#648=VERTEX_POINT('',#2261);
#649=VERTEX_POINT('',#2263);
#650=VERTEX_POINT('',#2265);
#651=VERTEX_POINT('',#2269);
#652=VERTEX_POINT('',#2271);
#653=VERTEX_POINT('',#2275);
#654=VERTEX_POINT('',#2277);
#655=VERTEX_POINT('',#2281);
#656=VERTEX_POINT('',#2282);
#657=VERTEX_POINT('',#2284);
#658=VERTEX_POINT('',#2286);
#659=VERTEX_POINT('',#2290);
#660=VERTEX_POINT('',#2292);
#661=VERTEX_POINT('',#2296);
#662=VERTEX_POINT('',#2297);
#663=VERTEX_POINT('',#2299);
#664=VERTEX_POINT('',#2301);
#665=VERTEX_POINT('',#2323);
#666=VERTEX_POINT('',#2325);
#667=VERTEX_POINT('',#2332);
#668=VERTEX_POINT('',#2333);
#669=VERTEX_POINT('',#2336);
#670=VERTEX_POINT('',#2340);
#671=VERTEX_POINT('',#2341);
#672=VERTEX_POINT('',#2343);
#673=VERTEX_POINT('',#2345);
#674=VERTEX_POINT('',#2347);
#675=VERTEX_POINT('',#2350);
#676=VERTEX_POINT('',#2352);
#677=VERTEX_POINT('',#2356);
#678=VERTEX_POINT('',#2358);
#679=VERTEX_POINT('',#2366);
#680=VERTEX_POINT('',#2370);
#681=VERTEX_POINT('',#2374);
#682=VERTEX_POINT('',#2378);
#683=VERTEX_POINT('',#2382);
#684=VERTEX_POINT('',#2386);
#685=VERTEX_POINT('',#2390);
#686=VERTEX_POINT('',#2391);
#687=VERTEX_POINT('',#2393);
#688=VERTEX_POINT('',#2395);
#689=VERTEX_POINT('',#2397);
#690=VERTEX_POINT('',#2399);
#691=VERTEX_POINT('',#2403);
#692=VERTEX_POINT('',#2411);
#693=VERTEX_POINT('',#2419);
#694=VERTEX_POINT('',#2427);
#695=VERTEX_POINT('',#2435);
#696=VERTEX_POINT('',#2443);
#697=EDGE_CURVE('',#570,#571,#276,.T.);
#698=EDGE_CURVE('',#572,#570,#277,.T.);
#699=EDGE_CURVE('',#572,#573,#278,.T.);
#700=EDGE_CURVE('',#571,#573,#279,.T.);
#701=EDGE_CURVE('',#574,#575,#280,.T.);
#702=EDGE_CURVE('',#576,#574,#281,.T.);
#703=EDGE_CURVE('',#576,#577,#282,.T.);
#704=EDGE_CURVE('',#575,#577,#283,.T.);
#705=EDGE_CURVE('',#578,#579,#284,.T.);
#706=EDGE_CURVE('',#580,#578,#285,.T.);
#707=EDGE_CURVE('',#580,#581,#286,.T.);
#708=EDGE_CURVE('',#581,#579,#287,.T.);
#709=EDGE_CURVE('',#582,#578,#288,.T.);
#710=EDGE_CURVE('',#583,#582,#289,.T.);
#711=EDGE_CURVE('',#583,#580,#290,.T.);
#712=EDGE_CURVE('',#584,#582,#291,.T.);
#713=EDGE_CURVE('',#585,#584,#292,.T.);
#714=EDGE_CURVE('',#585,#583,#293,.T.);
#715=EDGE_CURVE('',#573,#584,#294,.T.);
#716=EDGE_CURVE('',#586,#572,#295,.T.);
#717=EDGE_CURVE('',#587,#586,#296,.T.);
#718=EDGE_CURVE('',#587,#585,#297,.T.);
#719=EDGE_CURVE('',#588,#571,#298,.T.);
#720=EDGE_CURVE('',#589,#588,#299,.T.);
#721=EDGE_CURVE('',#589,#590,#300,.T.);
#722=EDGE_CURVE('',#591,#590,#301,.T.);
#723=EDGE_CURVE('',#591,#570,#302,.T.);
#724=EDGE_CURVE('',#592,#588,#303,.T.);
#725=EDGE_CURVE('',#593,#592,#304,.T.);
#726=EDGE_CURVE('',#593,#589,#305,.T.);
#727=EDGE_CURVE('',#594,#592,#306,.T.);
#728=EDGE_CURVE('',#595,#594,#307,.T.);
#729=EDGE_CURVE('',#595,#593,#308,.T.);
#730=EDGE_CURVE('',#596,#594,#309,.T.);
#731=EDGE_CURVE('',#597,#596,#310,.T.);
#732=EDGE_CURVE('',#597,#595,#311,.T.);
#733=EDGE_CURVE('',#598,#596,#312,.T.);
#734=EDGE_CURVE('',#599,#598,#313,.T.);
#735=EDGE_CURVE('',#599,#597,#314,.T.);
#736=EDGE_CURVE('',#600,#598,#315,.T.);
#737=EDGE_CURVE('',#601,#600,#316,.T.);
#738=EDGE_CURVE('',#601,#599,#317,.T.);
#739=EDGE_CURVE('',#577,#600,#318,.T.);
#740=EDGE_CURVE('',#602,#576,#319,.T.);
#741=EDGE_CURVE('',#603,#602,#320,.T.);
#742=EDGE_CURVE('',#603,#601,#321,.T.);
#743=EDGE_CURVE('',#604,#575,#322,.T.);
#744=EDGE_CURVE('',#605,#604,#323,.T.);
#745=EDGE_CURVE('',#605,#606,#324,.T.);
#746=EDGE_CURVE('',#607,#606,#325,.T.);
#747=EDGE_CURVE('',#607,#574,#326,.T.);
#748=EDGE_CURVE('',#608,#604,#327,.T.);
#749=EDGE_CURVE('',#609,#608,#328,.T.);
#750=EDGE_CURVE('',#609,#605,#329,.T.);
#751=EDGE_CURVE('',#610,#608,#330,.T.);
#752=EDGE_CURVE('',#611,#610,#331,.T.);
#753=EDGE_CURVE('',#611,#609,#332,.T.);
#754=EDGE_CURVE('',#612,#610,#333,.T.);
#755=EDGE_CURVE('',#613,#612,#334,.T.);
#756=EDGE_CURVE('',#613,#611,#335,.T.);
#757=EDGE_CURVE('',#614,#612,#336,.T.);
#758=EDGE_CURVE('',#615,#614,#337,.T.);
#759=EDGE_CURVE('',#615,#613,#338,.T.);
#760=EDGE_CURVE('',#616,#614,#339,.T.);
#761=EDGE_CURVE('',#617,#616,#340,.T.);
#762=EDGE_CURVE('',#617,#615,#341,.T.);
#763=EDGE_CURVE('',#618,#616,#342,.T.);
#764=EDGE_CURVE('',#619,#618,#343,.T.);
#765=EDGE_CURVE('',#619,#617,#344,.T.);
#766=EDGE_CURVE('',#620,#618,#345,.T.);
#767=EDGE_CURVE('',#621,#620,#346,.T.);
#768=EDGE_CURVE('',#621,#619,#347,.T.);
#769=EDGE_CURVE('',#579,#620,#348,.T.);
#770=EDGE_CURVE('',#581,#621,#349,.T.);
#771=EDGE_CURVE('',#590,#587,#350,.T.);
#772=EDGE_CURVE('',#606,#603,#351,.T.);
#773=EDGE_CURVE('',#602,#607,#352,.T.);
#774=EDGE_CURVE('',#586,#591,#353,.T.);
#775=EDGE_CURVE('',#622,#623,#86,.T.);
#776=EDGE_CURVE('',#623,#624,#354,.T.);
#777=EDGE_CURVE('',#624,#624,#50,.T.);
#778=EDGE_CURVE('',#623,#622,#87,.T.);
#779=EDGE_CURVE('',#625,#626,#355,.T.);
#780=EDGE_CURVE('',#627,#625,#356,.T.);
#781=EDGE_CURVE('',#627,#628,#357,.T.);
#782=EDGE_CURVE('',#628,#626,#358,.T.);
#783=EDGE_CURVE('',#629,#625,#359,.T.);
#784=EDGE_CURVE('',#630,#629,#360,.T.);
#785=EDGE_CURVE('',#630,#627,#361,.T.);
#786=EDGE_CURVE('',#631,#629,#51,.T.);
#787=EDGE_CURVE('',#632,#631,#362,.T.);
#788=EDGE_CURVE('',#632,#630,#52,.T.);
#789=EDGE_CURVE('',#633,#631,#363,.T.);
#790=EDGE_CURVE('',#634,#633,#364,.T.);
#791=EDGE_CURVE('',#634,#632,#365,.T.);
#792=EDGE_CURVE('',#635,#633,#366,.T.);
#793=EDGE_CURVE('',#636,#635,#367,.T.);
#794=EDGE_CURVE('',#636,#634,#368,.T.);
#795=EDGE_CURVE('',#637,#635,#369,.T.);
#796=EDGE_CURVE('',#638,#637,#370,.T.);
#797=EDGE_CURVE('',#638,#636,#371,.T.);
#798=EDGE_CURVE('',#639,#637,#372,.T.);
#799=EDGE_CURVE('',#639,#640,#373,.T.);
#800=EDGE_CURVE('',#640,#638,#374,.T.);
#801=EDGE_CURVE('',#641,#642,#375,.T.);
#802=EDGE_CURVE('',#642,#643,#376,.T.);
#803=EDGE_CURVE('',#644,#643,#377,.T.);
#804=EDGE_CURVE('',#641,#644,#378,.T.);
#805=EDGE_CURVE('',#645,#644,#53,.T.);
#806=EDGE_CURVE('',#645,#646,#379,.T.);
#807=EDGE_CURVE('',#646,#641,#54,.T.);
#808=EDGE_CURVE('',#647,#648,#380,.T.);
#809=EDGE_CURVE('',#648,#649,#381,.T.);
#810=EDGE_CURVE('',#650,#649,#382,.T.);
#811=EDGE_CURVE('',#647,#650,#383,.T.);
#812=EDGE_CURVE('',#651,#650,#384,.T.);
#813=EDGE_CURVE('',#652,#651,#385,.T.);
#814=EDGE_CURVE('',#652,#647,#386,.T.);
#815=EDGE_CURVE('',#653,#651,#387,.T.);
#816=EDGE_CURVE('',#653,#654,#388,.T.);
#817=EDGE_CURVE('',#654,#652,#389,.T.);
#818=EDGE_CURVE('',#655,#656,#55,.T.);
#819=EDGE_CURVE('',#656,#657,#390,.T.);
#820=EDGE_CURVE('',#658,#657,#56,.T.);
#821=EDGE_CURVE('',#655,#658,#391,.T.);
#822=EDGE_CURVE('',#659,#658,#392,.T.);
#823=EDGE_CURVE('',#659,#660,#393,.T.);
#824=EDGE_CURVE('',#660,#655,#394,.T.);
#825=EDGE_CURVE('',#661,#662,#395,.T.);
#826=EDGE_CURVE('',#662,#663,#396,.T.);
#827=EDGE_CURVE('',#664,#663,#397,.T.);
#828=EDGE_CURVE('',#661,#664,#398,.T.);
#829=EDGE_CURVE('',#626,#664,#399,.T.);
#830=EDGE_CURVE('',#628,#661,#400,.T.);
#831=EDGE_CURVE('',#660,#662,#57,.T.);
#832=EDGE_CURVE('',#640,#642,#58,.T.);
#833=EDGE_CURVE('',#646,#648,#59,.T.);
#834=EDGE_CURVE('',#654,#656,#60,.T.);
#835=EDGE_CURVE('',#663,#659,#61,.T.);
#836=EDGE_CURVE('',#657,#653,#62,.T.);
#837=EDGE_CURVE('',#649,#645,#63,.T.);
#838=EDGE_CURVE('',#643,#639,#64,.T.);
#839=EDGE_CURVE('',#665,#665,#65,.T.);
#840=EDGE_CURVE('',#665,#666,#401,.T.);
#841=EDGE_CURVE('',#666,#666,#66,.T.);
#842=EDGE_CURVE('',#667,#668,#67,.T.);
#843=EDGE_CURVE('',#668,#667,#68,.T.);
#844=EDGE_CURVE('',#668,#669,#69,.T.);
#845=EDGE_CURVE('',#669,#669,#70,.T.);
#846=EDGE_CURVE('',#670,#671,#71,.T.);
#847=EDGE_CURVE('',#672,#670,#72,.T.);
#848=EDGE_CURVE('',#673,#672,#73,.T.);
#849=EDGE_CURVE('',#673,#674,#402,.T.);
#850=EDGE_CURVE('',#674,#674,#74,.T.);
#851=EDGE_CURVE('',#675,#673,#75,.T.);
#852=EDGE_CURVE('',#676,#675,#76,.T.);
#853=EDGE_CURVE('',#671,#676,#77,.T.);
#854=EDGE_CURVE('',#677,#677,#78,.T.);
#855=EDGE_CURVE('',#677,#678,#403,.T.);
#856=EDGE_CURVE('',#678,#678,#79,.T.);
#857=EDGE_CURVE('',#667,#677,#404,.T.);
#858=EDGE_CURVE('',#679,#675,#405,.T.);
#859=EDGE_CURVE('',#673,#679,#406,.T.);
#860=EDGE_CURVE('',#675,#680,#407,.T.);
#861=EDGE_CURVE('',#680,#676,#408,.T.);
#862=EDGE_CURVE('',#676,#681,#409,.T.);
#863=EDGE_CURVE('',#681,#671,#410,.T.);
#864=EDGE_CURVE('',#671,#682,#411,.T.);
#865=EDGE_CURVE('',#682,#670,#412,.T.);
#866=EDGE_CURVE('',#670,#683,#413,.T.);
#867=EDGE_CURVE('',#683,#672,#414,.T.);
#868=EDGE_CURVE('',#672,#684,#415,.T.);
#869=EDGE_CURVE('',#684,#673,#416,.T.);
#870=EDGE_CURVE('',#685,#686,#80,.T.);
#871=EDGE_CURVE('',#687,#685,#81,.T.);
#872=EDGE_CURVE('',#688,#687,#82,.T.);
#873=EDGE_CURVE('',#689,#688,#83,.T.);
#874=EDGE_CURVE('',#689,#690,#84,.T.);
#875=EDGE_CURVE('',#686,#690,#85,.T.);
#876=EDGE_CURVE('',#690,#691,#27,.T.);
#877=EDGE_CURVE('',#691,#686,#28,.T.);
#878=EDGE_CURVE('',#689,#692,#29,.T.);
#879=EDGE_CURVE('',#692,#690,#30,.T.);
#880=EDGE_CURVE('',#693,#689,#31,.T.);
#881=EDGE_CURVE('',#688,#693,#32,.T.);
#882=EDGE_CURVE('',#694,#688,#33,.T.);
#883=EDGE_CURVE('',#687,#694,#34,.T.);
#884=EDGE_CURVE('',#686,#695,#35,.T.);
#885=EDGE_CURVE('',#695,#685,#36,.T.);
#886=EDGE_CURVE('',#696,#687,#37,.T.);
#887=EDGE_CURVE('',#685,#696,#38,.T.);
#888=EDGE_CURVE('',#684,#696,#417,.T.);
#889=EDGE_CURVE('',#679,#695,#418,.T.);
#890=EDGE_CURVE('',#683,#694,#419,.T.);
#891=EDGE_CURVE('',#682,#693,#420,.T.);
#892=EDGE_CURVE('',#681,#692,#421,.T.);
#893=EDGE_CURVE('',#680,#691,#422,.T.);
#894=ORIENTED_EDGE('',*,*,#697,.F.);
#895=ORIENTED_EDGE('',*,*,#698,.F.);
#896=ORIENTED_EDGE('',*,*,#699,.T.);
#897=ORIENTED_EDGE('',*,*,#700,.F.);
#898=ORIENTED_EDGE('',*,*,#701,.F.);
#899=ORIENTED_EDGE('',*,*,#702,.F.);
#900=ORIENTED_EDGE('',*,*,#703,.T.);
#901=ORIENTED_EDGE('',*,*,#704,.F.);
#902=ORIENTED_EDGE('',*,*,#705,.F.);
#903=ORIENTED_EDGE('',*,*,#706,.F.);
#904=ORIENTED_EDGE('',*,*,#707,.T.);
#905=ORIENTED_EDGE('',*,*,#708,.T.);
#906=ORIENTED_EDGE('',*,*,#709,.F.);
#907=ORIENTED_EDGE('',*,*,#710,.F.);
#908=ORIENTED_EDGE('',*,*,#711,.T.);
#909=ORIENTED_EDGE('',*,*,#706,.T.);
#910=ORIENTED_EDGE('',*,*,#712,.F.);
#911=ORIENTED_EDGE('',*,*,#713,.F.);
#912=ORIENTED_EDGE('',*,*,#714,.T.);
#913=ORIENTED_EDGE('',*,*,#710,.T.);
#914=ORIENTED_EDGE('',*,*,#715,.F.);
#915=ORIENTED_EDGE('',*,*,#699,.F.);
#916=ORIENTED_EDGE('',*,*,#716,.F.);
#917=ORIENTED_EDGE('',*,*,#717,.F.);
#918=ORIENTED_EDGE('',*,*,#718,.T.);
#919=ORIENTED_EDGE('',*,*,#713,.T.);
#920=ORIENTED_EDGE('',*,*,#719,.F.);
#921=ORIENTED_EDGE('',*,*,#720,.F.);
#922=ORIENTED_EDGE('',*,*,#721,.T.);
#923=ORIENTED_EDGE('',*,*,#722,.F.);
#924=ORIENTED_EDGE('',*,*,#723,.T.);
#925=ORIENTED_EDGE('',*,*,#697,.T.);
#926=ORIENTED_EDGE('',*,*,#724,.F.);
#927=ORIENTED_EDGE('',*,*,#725,.F.);
#928=ORIENTED_EDGE('',*,*,#726,.T.);
#929=ORIENTED_EDGE('',*,*,#720,.T.);
#930=ORIENTED_EDGE('',*,*,#727,.F.);
#931=ORIENTED_EDGE('',*,*,#728,.F.);
#932=ORIENTED_EDGE('',*,*,#729,.T.);
#933=ORIENTED_EDGE('',*,*,#725,.T.);
#934=ORIENTED_EDGE('',*,*,#730,.F.);
#935=ORIENTED_EDGE('',*,*,#731,.F.);
#936=ORIENTED_EDGE('',*,*,#732,.T.);
#937=ORIENTED_EDGE('',*,*,#728,.T.);
#938=ORIENTED_EDGE('',*,*,#733,.F.);
#939=ORIENTED_EDGE('',*,*,#734,.F.);
#940=ORIENTED_EDGE('',*,*,#735,.T.);
#941=ORIENTED_EDGE('',*,*,#731,.T.);
#942=ORIENTED_EDGE('',*,*,#736,.F.);
#943=ORIENTED_EDGE('',*,*,#737,.F.);
#944=ORIENTED_EDGE('',*,*,#738,.T.);
#945=ORIENTED_EDGE('',*,*,#734,.T.);
#946=ORIENTED_EDGE('',*,*,#739,.F.);
#947=ORIENTED_EDGE('',*,*,#703,.F.);
#948=ORIENTED_EDGE('',*,*,#740,.F.);
#949=ORIENTED_EDGE('',*,*,#741,.F.);
#950=ORIENTED_EDGE('',*,*,#742,.T.);
#951=ORIENTED_EDGE('',*,*,#737,.T.);
#952=ORIENTED_EDGE('',*,*,#743,.F.);
#953=ORIENTED_EDGE('',*,*,#744,.F.);
#954=ORIENTED_EDGE('',*,*,#745,.T.);
#955=ORIENTED_EDGE('',*,*,#746,.F.);
#956=ORIENTED_EDGE('',*,*,#747,.T.);
#957=ORIENTED_EDGE('',*,*,#701,.T.);
#958=ORIENTED_EDGE('',*,*,#748,.F.);
#959=ORIENTED_EDGE('',*,*,#749,.F.);
#960=ORIENTED_EDGE('',*,*,#750,.T.);
#961=ORIENTED_EDGE('',*,*,#744,.T.);
#962=ORIENTED_EDGE('',*,*,#751,.F.);
#963=ORIENTED_EDGE('',*,*,#752,.F.);
#964=ORIENTED_EDGE('',*,*,#753,.T.);
#965=ORIENTED_EDGE('',*,*,#749,.T.);
#966=ORIENTED_EDGE('',*,*,#754,.F.);
#967=ORIENTED_EDGE('',*,*,#755,.F.);
#968=ORIENTED_EDGE('',*,*,#756,.T.);
#969=ORIENTED_EDGE('',*,*,#752,.T.);
#970=ORIENTED_EDGE('',*,*,#757,.F.);
#971=ORIENTED_EDGE('',*,*,#758,.F.);
#972=ORIENTED_EDGE('',*,*,#759,.T.);
#973=ORIENTED_EDGE('',*,*,#755,.T.);
#974=ORIENTED_EDGE('',*,*,#760,.F.);
#975=ORIENTED_EDGE('',*,*,#761,.F.);
#976=ORIENTED_EDGE('',*,*,#762,.T.);
#977=ORIENTED_EDGE('',*,*,#758,.T.);
#978=ORIENTED_EDGE('',*,*,#763,.F.);
#979=ORIENTED_EDGE('',*,*,#764,.F.);
#980=ORIENTED_EDGE('',*,*,#765,.T.);
#981=ORIENTED_EDGE('',*,*,#761,.T.);
#982=ORIENTED_EDGE('',*,*,#766,.F.);
#983=ORIENTED_EDGE('',*,*,#767,.F.);
#984=ORIENTED_EDGE('',*,*,#768,.T.);
#985=ORIENTED_EDGE('',*,*,#764,.T.);
#986=ORIENTED_EDGE('',*,*,#769,.F.);
#987=ORIENTED_EDGE('',*,*,#708,.F.);
#988=ORIENTED_EDGE('',*,*,#770,.T.);
#989=ORIENTED_EDGE('',*,*,#767,.T.);
#990=ORIENTED_EDGE('',*,*,#707,.F.);
#991=ORIENTED_EDGE('',*,*,#711,.F.);
#992=ORIENTED_EDGE('',*,*,#714,.F.);
#993=ORIENTED_EDGE('',*,*,#718,.F.);
#994=ORIENTED_EDGE('',*,*,#771,.F.);
#995=ORIENTED_EDGE('',*,*,#721,.F.);
#996=ORIENTED_EDGE('',*,*,#726,.F.);
#997=ORIENTED_EDGE('',*,*,#729,.F.);
#998=ORIENTED_EDGE('',*,*,#732,.F.);
#999=ORIENTED_EDGE('',*,*,#735,.F.);
#1000=ORIENTED_EDGE('',*,*,#738,.F.);
#1001=ORIENTED_EDGE('',*,*,#742,.F.);
#1002=ORIENTED_EDGE('',*,*,#772,.F.);
#1003=ORIENTED_EDGE('',*,*,#745,.F.);
#1004=ORIENTED_EDGE('',*,*,#750,.F.);
#1005=ORIENTED_EDGE('',*,*,#753,.F.);
#1006=ORIENTED_EDGE('',*,*,#756,.F.);
#1007=ORIENTED_EDGE('',*,*,#759,.F.);
#1008=ORIENTED_EDGE('',*,*,#762,.F.);
#1009=ORIENTED_EDGE('',*,*,#765,.F.);
#1010=ORIENTED_EDGE('',*,*,#768,.F.);
#1011=ORIENTED_EDGE('',*,*,#770,.F.);
#1012=ORIENTED_EDGE('',*,*,#705,.T.);
#1013=ORIENTED_EDGE('',*,*,#769,.T.);
#1014=ORIENTED_EDGE('',*,*,#766,.T.);
#1015=ORIENTED_EDGE('',*,*,#763,.T.);
#1016=ORIENTED_EDGE('',*,*,#760,.T.);
#1017=ORIENTED_EDGE('',*,*,#757,.T.);
#1018=ORIENTED_EDGE('',*,*,#754,.T.);
#1019=ORIENTED_EDGE('',*,*,#751,.T.);
#1020=ORIENTED_EDGE('',*,*,#748,.T.);
#1021=ORIENTED_EDGE('',*,*,#743,.T.);
#1022=ORIENTED_EDGE('',*,*,#704,.T.);
#1023=ORIENTED_EDGE('',*,*,#739,.T.);
#1024=ORIENTED_EDGE('',*,*,#736,.T.);
#1025=ORIENTED_EDGE('',*,*,#733,.T.);
#1026=ORIENTED_EDGE('',*,*,#730,.T.);
#1027=ORIENTED_EDGE('',*,*,#727,.T.);
#1028=ORIENTED_EDGE('',*,*,#724,.T.);
#1029=ORIENTED_EDGE('',*,*,#719,.T.);
#1030=ORIENTED_EDGE('',*,*,#700,.T.);
#1031=ORIENTED_EDGE('',*,*,#715,.T.);
#1032=ORIENTED_EDGE('',*,*,#712,.T.);
#1033=ORIENTED_EDGE('',*,*,#709,.T.);
#1034=ORIENTED_EDGE('',*,*,#702,.T.);
#1035=ORIENTED_EDGE('',*,*,#747,.F.);
#1036=ORIENTED_EDGE('',*,*,#773,.F.);
#1037=ORIENTED_EDGE('',*,*,#740,.T.);
#1038=ORIENTED_EDGE('',*,*,#772,.T.);
#1039=ORIENTED_EDGE('',*,*,#741,.T.);
#1040=ORIENTED_EDGE('',*,*,#773,.T.);
#1041=ORIENTED_EDGE('',*,*,#746,.T.);
#1042=ORIENTED_EDGE('',*,*,#698,.T.);
#1043=ORIENTED_EDGE('',*,*,#723,.F.);
#1044=ORIENTED_EDGE('',*,*,#774,.F.);
#1045=ORIENTED_EDGE('',*,*,#716,.T.);
#1046=ORIENTED_EDGE('',*,*,#771,.T.);
#1047=ORIENTED_EDGE('',*,*,#717,.T.);
#1048=ORIENTED_EDGE('',*,*,#774,.T.);
#1049=ORIENTED_EDGE('',*,*,#722,.T.);
#1050=ORIENTED_EDGE('',*,*,#775,.T.);
#1051=ORIENTED_EDGE('',*,*,#776,.T.);
#1052=ORIENTED_EDGE('',*,*,#777,.T.);
#1053=ORIENTED_EDGE('',*,*,#776,.F.);
#1054=ORIENTED_EDGE('',*,*,#778,.T.);
#1055=ORIENTED_EDGE('',*,*,#779,.F.);
#1056=ORIENTED_EDGE('',*,*,#780,.F.);
#1057=ORIENTED_EDGE('',*,*,#781,.T.);
#1058=ORIENTED_EDGE('',*,*,#782,.T.);
#1059=ORIENTED_EDGE('',*,*,#783,.F.);
#1060=ORIENTED_EDGE('',*,*,#784,.F.);
#1061=ORIENTED_EDGE('',*,*,#785,.T.);
#1062=ORIENTED_EDGE('',*,*,#780,.T.);
#1063=ORIENTED_EDGE('',*,*,#786,.F.);
#1064=ORIENTED_EDGE('',*,*,#787,.F.);
#1065=ORIENTED_EDGE('',*,*,#788,.T.);
#1066=ORIENTED_EDGE('',*,*,#784,.T.);
#1067=ORIENTED_EDGE('',*,*,#775,.F.);
#1068=ORIENTED_EDGE('',*,*,#778,.F.);
#1069=ORIENTED_EDGE('',*,*,#789,.F.);
#1070=ORIENTED_EDGE('',*,*,#790,.F.);
#1071=ORIENTED_EDGE('',*,*,#791,.T.);
#1072=ORIENTED_EDGE('',*,*,#787,.T.);
#1073=ORIENTED_EDGE('',*,*,#792,.F.);
#1074=ORIENTED_EDGE('',*,*,#793,.F.);
#1075=ORIENTED_EDGE('',*,*,#794,.T.);
#1076=ORIENTED_EDGE('',*,*,#790,.T.);
#1077=ORIENTED_EDGE('',*,*,#795,.F.);
#1078=ORIENTED_EDGE('',*,*,#796,.F.);
#1079=ORIENTED_EDGE('',*,*,#797,.T.);
#1080=ORIENTED_EDGE('',*,*,#793,.T.);
#1081=ORIENTED_EDGE('',*,*,#798,.F.);
#1082=ORIENTED_EDGE('',*,*,#799,.T.);
#1083=ORIENTED_EDGE('',*,*,#800,.T.);
#1084=ORIENTED_EDGE('',*,*,#796,.T.);
#1085=ORIENTED_EDGE('',*,*,#801,.T.);
#1086=ORIENTED_EDGE('',*,*,#802,.T.);
#1087=ORIENTED_EDGE('',*,*,#803,.F.);
#1088=ORIENTED_EDGE('',*,*,#804,.F.);
#1089=ORIENTED_EDGE('',*,*,#805,.F.);
#1090=ORIENTED_EDGE('',*,*,#806,.T.);
#1091=ORIENTED_EDGE('',*,*,#807,.T.);
#1092=ORIENTED_EDGE('',*,*,#804,.T.);
#1093=ORIENTED_EDGE('',*,*,#808,.T.);
#1094=ORIENTED_EDGE('',*,*,#809,.T.);
#1095=ORIENTED_EDGE('',*,*,#810,.F.);
#1096=ORIENTED_EDGE('',*,*,#811,.F.);
#1097=ORIENTED_EDGE('',*,*,#812,.F.);
#1098=ORIENTED_EDGE('',*,*,#813,.F.);
#1099=ORIENTED_EDGE('',*,*,#814,.T.);
#1100=ORIENTED_EDGE('',*,*,#811,.T.);
#1101=ORIENTED_EDGE('',*,*,#777,.F.);
#1102=ORIENTED_EDGE('',*,*,#815,.F.);
#1103=ORIENTED_EDGE('',*,*,#816,.T.);
#1104=ORIENTED_EDGE('',*,*,#817,.T.);
#1105=ORIENTED_EDGE('',*,*,#813,.T.);
#1106=ORIENTED_EDGE('',*,*,#818,.T.);
#1107=ORIENTED_EDGE('',*,*,#819,.T.);
#1108=ORIENTED_EDGE('',*,*,#820,.F.);
#1109=ORIENTED_EDGE('',*,*,#821,.F.);
#1110=ORIENTED_EDGE('',*,*,#822,.F.);
#1111=ORIENTED_EDGE('',*,*,#823,.T.);
#1112=ORIENTED_EDGE('',*,*,#824,.T.);
#1113=ORIENTED_EDGE('',*,*,#821,.T.);
#1114=ORIENTED_EDGE('',*,*,#825,.T.);
#1115=ORIENTED_EDGE('',*,*,#826,.T.);
#1116=ORIENTED_EDGE('',*,*,#827,.F.);
#1117=ORIENTED_EDGE('',*,*,#828,.F.);
#1118=ORIENTED_EDGE('',*,*,#829,.F.);
#1119=ORIENTED_EDGE('',*,*,#782,.F.);
#1120=ORIENTED_EDGE('',*,*,#830,.T.);
#1121=ORIENTED_EDGE('',*,*,#828,.T.);
#1122=ORIENTED_EDGE('',*,*,#824,.F.);
#1123=ORIENTED_EDGE('',*,*,#831,.T.);
#1124=ORIENTED_EDGE('',*,*,#825,.F.);
#1125=ORIENTED_EDGE('',*,*,#830,.F.);
#1126=ORIENTED_EDGE('',*,*,#781,.F.);
#1127=ORIENTED_EDGE('',*,*,#785,.F.);
#1128=ORIENTED_EDGE('',*,*,#788,.F.);
#1129=ORIENTED_EDGE('',*,*,#791,.F.);
#1130=ORIENTED_EDGE('',*,*,#794,.F.);
#1131=ORIENTED_EDGE('',*,*,#797,.F.);
#1132=ORIENTED_EDGE('',*,*,#800,.F.);
#1133=ORIENTED_EDGE('',*,*,#832,.T.);
#1134=ORIENTED_EDGE('',*,*,#801,.F.);
#1135=ORIENTED_EDGE('',*,*,#807,.F.);
#1136=ORIENTED_EDGE('',*,*,#833,.T.);
#1137=ORIENTED_EDGE('',*,*,#808,.F.);
#1138=ORIENTED_EDGE('',*,*,#814,.F.);
#1139=ORIENTED_EDGE('',*,*,#817,.F.);
#1140=ORIENTED_EDGE('',*,*,#834,.T.);
#1141=ORIENTED_EDGE('',*,*,#818,.F.);
#1142=ORIENTED_EDGE('',*,*,#827,.T.);
#1143=ORIENTED_EDGE('',*,*,#835,.T.);
#1144=ORIENTED_EDGE('',*,*,#822,.T.);
#1145=ORIENTED_EDGE('',*,*,#820,.T.);
#1146=ORIENTED_EDGE('',*,*,#836,.T.);
#1147=ORIENTED_EDGE('',*,*,#815,.T.);
#1148=ORIENTED_EDGE('',*,*,#812,.T.);
#1149=ORIENTED_EDGE('',*,*,#810,.T.);
#1150=ORIENTED_EDGE('',*,*,#837,.T.);
#1151=ORIENTED_EDGE('',*,*,#805,.T.);
#1152=ORIENTED_EDGE('',*,*,#803,.T.);
#1153=ORIENTED_EDGE('',*,*,#838,.T.);
#1154=ORIENTED_EDGE('',*,*,#798,.T.);
#1155=ORIENTED_EDGE('',*,*,#795,.T.);
#1156=ORIENTED_EDGE('',*,*,#792,.T.);
#1157=ORIENTED_EDGE('',*,*,#789,.T.);
#1158=ORIENTED_EDGE('',*,*,#786,.T.);
#1159=ORIENTED_EDGE('',*,*,#783,.T.);
#1160=ORIENTED_EDGE('',*,*,#779,.T.);
#1161=ORIENTED_EDGE('',*,*,#829,.T.);
#1162=ORIENTED_EDGE('',*,*,#831,.F.);
#1163=ORIENTED_EDGE('',*,*,#823,.F.);
#1164=ORIENTED_EDGE('',*,*,#835,.F.);
#1165=ORIENTED_EDGE('',*,*,#826,.F.);
#1166=ORIENTED_EDGE('',*,*,#832,.F.);
#1167=ORIENTED_EDGE('',*,*,#799,.F.);
#1168=ORIENTED_EDGE('',*,*,#838,.F.);
#1169=ORIENTED_EDGE('',*,*,#802,.F.);
#1170=ORIENTED_EDGE('',*,*,#833,.F.);
#1171=ORIENTED_EDGE('',*,*,#806,.F.);
#1172=ORIENTED_EDGE('',*,*,#837,.F.);
#1173=ORIENTED_EDGE('',*,*,#809,.F.);
#1174=ORIENTED_EDGE('',*,*,#834,.F.);
#1175=ORIENTED_EDGE('',*,*,#816,.F.);
#1176=ORIENTED_EDGE('',*,*,#836,.F.);
#1177=ORIENTED_EDGE('',*,*,#819,.F.);
#1178=ORIENTED_EDGE('',*,*,#839,.F.);
#1179=ORIENTED_EDGE('',*,*,#840,.T.);
#1180=ORIENTED_EDGE('',*,*,#841,.T.);
#1181=ORIENTED_EDGE('',*,*,#840,.F.);
#1182=ORIENTED_EDGE('',*,*,#841,.F.);
#1183=ORIENTED_EDGE('',*,*,#839,.T.);
#1184=ORIENTED_EDGE('',*,*,#842,.F.);
#1185=ORIENTED_EDGE('',*,*,#843,.F.);
#1186=ORIENTED_EDGE('',*,*,#844,.T.);
#1187=ORIENTED_EDGE('',*,*,#845,.F.);
#1188=ORIENTED_EDGE('',*,*,#844,.F.);
#1189=ORIENTED_EDGE('',*,*,#846,.F.);
#1190=ORIENTED_EDGE('',*,*,#847,.F.);
#1191=ORIENTED_EDGE('',*,*,#848,.F.);
#1192=ORIENTED_EDGE('',*,*,#849,.T.);
#1193=ORIENTED_EDGE('',*,*,#850,.F.);
#1194=ORIENTED_EDGE('',*,*,#849,.F.);
#1195=ORIENTED_EDGE('',*,*,#851,.F.);
#1196=ORIENTED_EDGE('',*,*,#852,.F.);
#1197=ORIENTED_EDGE('',*,*,#853,.F.);
#1198=ORIENTED_EDGE('',*,*,#854,.F.);
#1199=ORIENTED_EDGE('',*,*,#855,.T.);
#1200=ORIENTED_EDGE('',*,*,#856,.T.);
#1201=ORIENTED_EDGE('',*,*,#855,.F.);
#1202=ORIENTED_EDGE('',*,*,#842,.T.);
#1203=ORIENTED_EDGE('',*,*,#843,.T.);
#1204=ORIENTED_EDGE('',*,*,#857,.T.);
#1205=ORIENTED_EDGE('',*,*,#854,.T.);
#1206=ORIENTED_EDGE('',*,*,#857,.F.);
#1207=ORIENTED_EDGE('',*,*,#850,.T.);
#1208=ORIENTED_EDGE('',*,*,#845,.T.);
#1209=ORIENTED_EDGE('',*,*,#856,.F.);
#1210=ORIENTED_EDGE('',*,*,#858,.T.);
#1211=ORIENTED_EDGE('',*,*,#851,.T.);
#1212=ORIENTED_EDGE('',*,*,#859,.T.);
#1213=ORIENTED_EDGE('',*,*,#860,.T.);
#1214=ORIENTED_EDGE('',*,*,#861,.T.);
#1215=ORIENTED_EDGE('',*,*,#852,.T.);
#1216=ORIENTED_EDGE('',*,*,#862,.T.);
#1217=ORIENTED_EDGE('',*,*,#863,.T.);
#1218=ORIENTED_EDGE('',*,*,#853,.T.);
#1219=ORIENTED_EDGE('',*,*,#864,.T.);
#1220=ORIENTED_EDGE('',*,*,#865,.T.);
#1221=ORIENTED_EDGE('',*,*,#846,.T.);
#1222=ORIENTED_EDGE('',*,*,#866,.T.);
#1223=ORIENTED_EDGE('',*,*,#867,.T.);
#1224=ORIENTED_EDGE('',*,*,#847,.T.);
#1225=ORIENTED_EDGE('',*,*,#868,.T.);
#1226=ORIENTED_EDGE('',*,*,#869,.T.);
#1227=ORIENTED_EDGE('',*,*,#848,.T.);
#1228=ORIENTED_EDGE('',*,*,#870,.F.);
#1229=ORIENTED_EDGE('',*,*,#871,.F.);
#1230=ORIENTED_EDGE('',*,*,#872,.F.);
#1231=ORIENTED_EDGE('',*,*,#873,.F.);
#1232=ORIENTED_EDGE('',*,*,#874,.T.);
#1233=ORIENTED_EDGE('',*,*,#875,.F.);
#1234=ORIENTED_EDGE('',*,*,#876,.T.);
#1235=ORIENTED_EDGE('',*,*,#877,.T.);
#1236=ORIENTED_EDGE('',*,*,#875,.T.);
#1237=ORIENTED_EDGE('',*,*,#878,.T.);
#1238=ORIENTED_EDGE('',*,*,#879,.T.);
#1239=ORIENTED_EDGE('',*,*,#874,.F.);
#1240=ORIENTED_EDGE('',*,*,#880,.T.);
#1241=ORIENTED_EDGE('',*,*,#873,.T.);
#1242=ORIENTED_EDGE('',*,*,#881,.T.);
#1243=ORIENTED_EDGE('',*,*,#882,.T.);
#1244=ORIENTED_EDGE('',*,*,#872,.T.);
#1245=ORIENTED_EDGE('',*,*,#883,.T.);
#1246=ORIENTED_EDGE('',*,*,#884,.T.);
#1247=ORIENTED_EDGE('',*,*,#885,.T.);
#1248=ORIENTED_EDGE('',*,*,#870,.T.);
#1249=ORIENTED_EDGE('',*,*,#886,.T.);
#1250=ORIENTED_EDGE('',*,*,#871,.T.);
#1251=ORIENTED_EDGE('',*,*,#887,.T.);
#1252=ORIENTED_EDGE('',*,*,#869,.F.);
#1253=ORIENTED_EDGE('',*,*,#888,.T.);
#1254=ORIENTED_EDGE('',*,*,#887,.F.);
#1255=ORIENTED_EDGE('',*,*,#885,.F.);
#1256=ORIENTED_EDGE('',*,*,#889,.F.);
#1257=ORIENTED_EDGE('',*,*,#859,.F.);
#1258=ORIENTED_EDGE('',*,*,#867,.F.);
#1259=ORIENTED_EDGE('',*,*,#890,.T.);
#1260=ORIENTED_EDGE('',*,*,#883,.F.);
#1261=ORIENTED_EDGE('',*,*,#886,.F.);
#1262=ORIENTED_EDGE('',*,*,#888,.F.);
#1263=ORIENTED_EDGE('',*,*,#868,.F.);
#1264=ORIENTED_EDGE('',*,*,#865,.F.);
#1265=ORIENTED_EDGE('',*,*,#891,.T.);
#1266=ORIENTED_EDGE('',*,*,#881,.F.);
#1267=ORIENTED_EDGE('',*,*,#882,.F.);
#1268=ORIENTED_EDGE('',*,*,#890,.F.);
#1269=ORIENTED_EDGE('',*,*,#866,.F.);
#1270=ORIENTED_EDGE('',*,*,#863,.F.);
#1271=ORIENTED_EDGE('',*,*,#892,.T.);
#1272=ORIENTED_EDGE('',*,*,#878,.F.);
#1273=ORIENTED_EDGE('',*,*,#880,.F.);
#1274=ORIENTED_EDGE('',*,*,#891,.F.);
#1275=ORIENTED_EDGE('',*,*,#864,.F.);
#1276=ORIENTED_EDGE('',*,*,#861,.F.);
#1277=ORIENTED_EDGE('',*,*,#893,.T.);
#1278=ORIENTED_EDGE('',*,*,#876,.F.);
#1279=ORIENTED_EDGE('',*,*,#879,.F.);
#1280=ORIENTED_EDGE('',*,*,#892,.F.);
#1281=ORIENTED_EDGE('',*,*,#862,.F.);
#1282=ORIENTED_EDGE('',*,*,#858,.F.);
#1283=ORIENTED_EDGE('',*,*,#889,.T.);
#1284=ORIENTED_EDGE('',*,*,#884,.F.);
#1285=ORIENTED_EDGE('',*,*,#877,.F.);
#1286=ORIENTED_EDGE('',*,*,#893,.F.);
#1287=ORIENTED_EDGE('',*,*,#860,.F.);
#1288=PLANE('',#1478);
#1289=PLANE('',#1479);
#1290=PLANE('',#1480);
#1291=PLANE('',#1481);
#1292=PLANE('',#1482);
#1293=PLANE('',#1483);
#1294=PLANE('',#1484);
#1295=PLANE('',#1485);
#1296=PLANE('',#1486);
#1297=PLANE('',#1487);
#1298=PLANE('',#1488);
#1299=PLANE('',#1489);
#1300=PLANE('',#1490);
#1301=PLANE('',#1491);
#1302=PLANE('',#1492);
#1303=PLANE('',#1493);
#1304=PLANE('',#1494);
#1305=PLANE('',#1495);
#1306=PLANE('',#1496);
#1307=PLANE('',#1497);
#1308=PLANE('',#1498);
#1309=PLANE('',#1499);
#1310=PLANE('',#1500);
#1311=PLANE('',#1501);
#1312=PLANE('',#1502);
#1313=PLANE('',#1503);
#1314=PLANE('',#1504);
#1315=PLANE('',#1505);
#1316=PLANE('',#1509);
#1317=PLANE('',#1510);
#1318=PLANE('',#1514);
#1319=PLANE('',#1515);
#1320=PLANE('',#1516);
#1321=PLANE('',#1517);
#1322=PLANE('',#1518);
#1323=PLANE('',#1522);
#1324=PLANE('',#1523);
#1325=PLANE('',#1524);
#1326=PLANE('',#1528);
#1327=PLANE('',#1529);
#1328=PLANE('',#1530);
#1329=PLANE('',#1531);
#1330=PLANE('',#1536);
#1331=PLANE('',#1549);
#1332=PLANE('',#1550);
#1333=PLANE('',#1569);
#1334=PLANE('',#1570);
#1335=PLANE('',#1571);
#1336=PLANE('',#1572);
#1337=PLANE('',#1573);
#1338=PLANE('',#1574);
#1339=PLANE('',#1575);
#1340=PLANE('',#1576);
#1341=PLANE('',#1577);
#1342=PLANE('',#1590);
#1343=PLANE('',#1591);
#1344=PLANE('',#1592);
#1345=PLANE('',#1593);
#1346=PLANE('',#1594);
#1347=PLANE('',#1595);
#1348=ADVANCED_FACE('',(#115),#1288,.T.);
#1349=ADVANCED_FACE('',(#116),#1289,.T.);
#1350=ADVANCED_FACE('',(#117),#1290,.T.);
#1351=ADVANCED_FACE('',(#118),#1291,.T.);
#1352=ADVANCED_FACE('',(#119),#1292,.T.);
#1353=ADVANCED_FACE('',(#120),#1293,.T.);
#1354=ADVANCED_FACE('',(#121),#1294,.T.);
#1355=ADVANCED_FACE('',(#122),#1295,.T.);
#1356=ADVANCED_FACE('',(#123),#1296,.T.);
#1357=ADVANCED_FACE('',(#124),#1297,.T.);
#1358=ADVANCED_FACE('',(#125),#1298,.T.);
#1359=ADVANCED_FACE('',(#126),#1299,.T.);
#1360=ADVANCED_FACE('',(#127),#1300,.T.);
#1361=ADVANCED_FACE('',(#128),#1301,.T.);
#1362=ADVANCED_FACE('',(#129),#1302,.T.);
#1363=ADVANCED_FACE('',(#130),#1303,.T.);
#1364=ADVANCED_FACE('',(#131),#1304,.T.);
#1365=ADVANCED_FACE('',(#132),#1305,.T.);
#1366=ADVANCED_FACE('',(#133),#1306,.T.);
#1367=ADVANCED_FACE('',(#134),#1307,.T.);
#1368=ADVANCED_FACE('',(#135),#1308,.T.);
#1369=ADVANCED_FACE('',(#136),#1309,.T.);
#1370=ADVANCED_FACE('',(#137),#1310,.T.);
#1371=ADVANCED_FACE('',(#138),#1311,.F.);
#1372=ADVANCED_FACE('',(#139),#1312,.F.);
#1373=ADVANCED_FACE('',(#140),#1313,.T.);
#1374=ADVANCED_FACE('',(#141),#1314,.F.);
#1375=ADVANCED_FACE('',(#142),#1315,.F.);
#1376=ADVANCED_FACE('',(#143),#88,.F.);
#1377=ADVANCED_FACE('',(#144),#1316,.T.);
#1378=ADVANCED_FACE('',(#145),#1317,.T.);
#1379=ADVANCED_FACE('',(#146,#47),#89,.F.);
#1380=ADVANCED_FACE('',(#147),#1318,.T.);
#1381=ADVANCED_FACE('',(#148),#1319,.T.);
#1382=ADVANCED_FACE('',(#149),#1320,.T.);
#1383=ADVANCED_FACE('',(#150),#1321,.T.);
#1384=ADVANCED_FACE('',(#151),#1322,.T.);
#1385=ADVANCED_FACE('',(#152),#90,.T.);
#1386=ADVANCED_FACE('',(#153),#1323,.T.);
#1387=ADVANCED_FACE('',(#154,#48),#1324,.T.);
#1388=ADVANCED_FACE('',(#155),#1325,.T.);
#1389=ADVANCED_FACE('',(#156),#91,.T.);
#1390=ADVANCED_FACE('',(#157),#1326,.T.);
#1391=ADVANCED_FACE('',(#158),#1327,.T.);
#1392=ADVANCED_FACE('',(#159),#1328,.T.);
#1393=ADVANCED_FACE('',(#160),#1329,.F.);
#1394=ADVANCED_FACE('',(#161),#1330,.T.);
#1395=ADVANCED_FACE('',(#162),#92,.T.);
#1396=ADVANCED_FACE('',(#163),#93,.T.);
#1397=ADVANCED_FACE('',(#164),#94,.F.);
#1398=ADVANCED_FACE('',(#165),#95,.F.);
#1399=ADVANCED_FACE('',(#166),#96,.T.);
#1400=ADVANCED_FACE('',(#167),#1331,.F.);
#1401=ADVANCED_FACE('',(#168),#1332,.T.);
#1402=ADVANCED_FACE('',(#169),#46,.F.);
#1403=ADVANCED_FACE('',(#170),#97,.T.);
#1404=ADVANCED_FACE('',(#171),#39,.T.);
#1405=ADVANCED_FACE('',(#172),#98,.T.);
#1406=ADVANCED_FACE('',(#173,#49),#1333,.T.);
#1407=ADVANCED_FACE('',(#174),#1334,.F.);
#1408=ADVANCED_FACE('',(#175),#1335,.T.);
#1409=ADVANCED_FACE('',(#176),#1336,.T.);
#1410=ADVANCED_FACE('',(#177),#1337,.T.);
#1411=ADVANCED_FACE('',(#178),#1338,.T.);
#1412=ADVANCED_FACE('',(#179),#1339,.T.);
#1413=ADVANCED_FACE('',(#180),#1340,.T.);
#1414=ADVANCED_FACE('',(#181),#1341,.F.);
#1415=ADVANCED_FACE('',(#182),#40,.T.);
#1416=ADVANCED_FACE('',(#183),#41,.T.);
#1417=ADVANCED_FACE('',(#184),#42,.T.);
#1418=ADVANCED_FACE('',(#185),#43,.T.);
#1419=ADVANCED_FACE('',(#186),#44,.T.);
#1420=ADVANCED_FACE('',(#187),#45,.T.);
#1421=ADVANCED_FACE('',(#188),#1342,.F.);
#1422=ADVANCED_FACE('',(#189),#1343,.F.);
#1423=ADVANCED_FACE('',(#190),#1344,.F.);
#1424=ADVANCED_FACE('',(#191),#1345,.F.);
#1425=ADVANCED_FACE('',(#192),#1346,.F.);
#1426=ADVANCED_FACE('',(#193),#1347,.F.);
#1427=CLOSED_SHELL('',(#1348,#1349,#1350,#1351,#1352,#1353,#1354,#1355,
#1356,#1357,#1358,#1359,#1360,#1361,#1362,#1363,#1364,#1365,#1366,#1367,
#1368,#1369,#1370,#1371,#1372,#1373,#1374,#1375));
#1428=CLOSED_SHELL('',(#1376,#1377,#1378,#1379,#1380,#1381,#1382,#1383,
#1384,#1385,#1386,#1387,#1388,#1389,#1390,#1391,#1392,#1393,#1394,#1395,
#1396,#1397,#1398));
#1429=CLOSED_SHELL('',(#1399,#1400,#1401));
#1430=CLOSED_SHELL('',(#1402,#1403,#1404,#1405,#1406,#1407,#1408,#1409,
#1410,#1411,#1412,#1413,#1414,#1415,#1416,#1417,#1418,#1419,#1420,#1421,
#1422,#1423,#1424,#1425,#1426));
#1431=DERIVED_UNIT_ELEMENT(#1439,1.);
#1432=DERIVED_UNIT_ELEMENT(#2479,-3.);
#1433=DERIVED_UNIT_ELEMENT(#1439,1.);
#1434=DERIVED_UNIT_ELEMENT(#2479,-3.);
#1435=DERIVED_UNIT_ELEMENT(#1439,1.);
#1436=DERIVED_UNIT_ELEMENT(#2479,-3.);
#1437=DERIVED_UNIT_ELEMENT(#1439,1.);
#1438=DERIVED_UNIT_ELEMENT(#2479,-3.);
#1439=(
MASS_UNIT()
NAMED_UNIT(*)
SI_UNIT(.KILO.,.GRAM.)
);
#1440=DERIVED_UNIT((#1431,#1432));
#1441=DERIVED_UNIT((#1433,#1434));
#1442=DERIVED_UNIT((#1435,#1436));
#1443=DERIVED_UNIT((#1437,#1438));
#1444=MEASURE_REPRESENTATION_ITEM('density measure',
POSITIVE_RATIO_MEASURE(7850.),#1440);
#1445=MEASURE_REPRESENTATION_ITEM('density measure',
POSITIVE_RATIO_MEASURE(7850.),#1441);
#1446=MEASURE_REPRESENTATION_ITEM('density measure',
POSITIVE_RATIO_MEASURE(7850.),#1442);
#1447=MEASURE_REPRESENTATION_ITEM('density measure',
POSITIVE_RATIO_MEASURE(7850.),#1443);
#1448=PROPERTY_DEFINITION_REPRESENTATION(#1468,#1456);
#1449=PROPERTY_DEFINITION_REPRESENTATION(#1469,#1457);
#1450=PROPERTY_DEFINITION_REPRESENTATION(#1470,#1458);
#1451=PROPERTY_DEFINITION_REPRESENTATION(#1471,#1459);
#1452=PROPERTY_DEFINITION_REPRESENTATION(#1472,#1460);
#1453=PROPERTY_DEFINITION_REPRESENTATION(#1473,#1461);
#1454=PROPERTY_DEFINITION_REPRESENTATION(#1474,#1462);
#1455=PROPERTY_DEFINITION_REPRESENTATION(#1475,#1463);
#1456=REPRESENTATION('material name',(#1464),#2473);
#1457=REPRESENTATION('density',(#1444),#2473);
#1458=REPRESENTATION('material name',(#1465),#2474);
#1459=REPRESENTATION('density',(#1445),#2474);
#1460=REPRESENTATION('material name',(#1466),#2475);
#1461=REPRESENTATION('density',(#1446),#2475);
#1462=REPRESENTATION('material name',(#1467),#2476);
#1463=REPRESENTATION('density',(#1447),#2476);
#1464=DESCRIPTIVE_REPRESENTATION_ITEM('Steel','Steel');
#1465=DESCRIPTIVE_REPRESENTATION_ITEM('Steel','Steel');
#1466=DESCRIPTIVE_REPRESENTATION_ITEM('Steel','Steel');
#1467=DESCRIPTIVE_REPRESENTATION_ITEM('Steel','Steel');
#1468=PROPERTY_DEFINITION('material property','material name',#2503);
#1469=PROPERTY_DEFINITION('material property','density of part',#2503);
#1470=PROPERTY_DEFINITION('material property','material name',#2504);
#1471=PROPERTY_DEFINITION('material property','density of part',#2504);
#1472=PROPERTY_DEFINITION('material property','material name',#2505);
#1473=PROPERTY_DEFINITION('material property','density of part',#2505);
#1474=PROPERTY_DEFINITION('material property','material name',#2506);
#1475=PROPERTY_DEFINITION('material property','density of part',#2506);
#1476=AXIS2_PLACEMENT_3D('',#1995,#1600,#1601);
#1477=AXIS2_PLACEMENT_3D('',#1996,#1602,#1603);
#1478=AXIS2_PLACEMENT_3D('',#1997,#1604,#1605);
#1479=AXIS2_PLACEMENT_3D('',#2006,#1610,#1611);
#1480=AXIS2_PLACEMENT_3D('',#2015,#1616,#1617);
#1481=AXIS2_PLACEMENT_3D('',#2024,#1622,#1623);
#1482=AXIS2_PLACEMENT_3D('',#2030,#1627,#1628);
#1483=AXIS2_PLACEMENT_3D('',#2036,#1632,#1633);
#1484=AXIS2_PLACEMENT_3D('',#2043,#1638,#1639);
#1485=AXIS2_PLACEMENT_3D('',#2053,#1645,#1646);
#1486=AXIS2_PLACEMENT_3D('',#2059,#1650,#1651);
#1487=AXIS2_PLACEMENT_3D('',#2065,#1655,#1656);
#1488=AXIS2_PLACEMENT_3D('',#2071,#1660,#1661);
#1489=AXIS2_PLACEMENT_3D('',#2077,#1665,#1666);
#1490=AXIS2_PLACEMENT_3D('',#2083,#1670,#1671);
#1491=AXIS2_PLACEMENT_3D('',#2090,#1676,#1677);
#1492=AXIS2_PLACEMENT_3D('',#2100,#1683,#1684);
#1493=AXIS2_PLACEMENT_3D('',#2106,#1688,#1689);
#1494=AXIS2_PLACEMENT_3D('',#2112,#1693,#1694);
#1495=AXIS2_PLACEMENT_3D('',#2118,#1698,#1699);
#1496=AXIS2_PLACEMENT_3D('',#2124,#1703,#1704);
#1497=AXIS2_PLACEMENT_3D('',#2130,#1708,#1709);
#1498=AXIS2_PLACEMENT_3D('',#2136,#1713,#1714);
#1499=AXIS2_PLACEMENT_3D('',#2142,#1718,#1719);
#1500=AXIS2_PLACEMENT_3D('',#2145,#1722,#1723);
#1501=AXIS2_PLACEMENT_3D('',#2148,#1726,#1727);
#1502=AXIS2_PLACEMENT_3D('',#2149,#1728,#1729);
#1503=AXIS2_PLACEMENT_3D('',#2151,#1731,#1732);
#1504=AXIS2_PLACEMENT_3D('',#2152,#1733,#1734);
#1505=AXIS2_PLACEMENT_3D('',#2154,#1736,#1737);
#1506=AXIS2_PLACEMENT_3D('',#2155,#1738,#1739);
#1507=AXIS2_PLACEMENT_3D('',#2156,#1740,#1741);
#1508=AXIS2_PLACEMENT_3D('',#2180,#1743,#1744);
#1509=AXIS2_PLACEMENT_3D('',#2199,#1745,#1746);
#1510=AXIS2_PLACEMENT_3D('',#2208,#1751,#1752);
#1511=AXIS2_PLACEMENT_3D('',#2214,#1756,#1757);
#1512=AXIS2_PLACEMENT_3D('',#2216,#1758,#1759);
#1513=AXIS2_PLACEMENT_3D('',#2219,#1761,#1762);
#1514=AXIS2_PLACEMENT_3D('',#2220,#1763,#1764);
#1515=AXIS2_PLACEMENT_3D('',#2226,#1768,#1769);
#1516=AXIS2_PLACEMENT_3D('',#2232,#1773,#1774);
#1517=AXIS2_PLACEMENT_3D('',#2238,#1778,#1779);
#1518=AXIS2_PLACEMENT_3D('',#2244,#1783,#1784);
#1519=AXIS2_PLACEMENT_3D('',#2253,#1789,#1790);
#1520=AXIS2_PLACEMENT_3D('',#2255,#1791,#1792);
#1521=AXIS2_PLACEMENT_3D('',#2258,#1794,#1795);
#1522=AXIS2_PLACEMENT_3D('',#2259,#1796,#1797);
#1523=AXIS2_PLACEMENT_3D('',#2268,#1802,#1803);
#1524=AXIS2_PLACEMENT_3D('',#2274,#1807,#1808);
#1525=AXIS2_PLACEMENT_3D('',#2280,#1812,#1813);
#1526=AXIS2_PLACEMENT_3D('',#2283,#1814,#1815);
#1527=AXIS2_PLACEMENT_3D('',#2287,#1817,#1818);
#1528=AXIS2_PLACEMENT_3D('',#2289,#1820,#1821);
#1529=AXIS2_PLACEMENT_3D('',#2295,#1825,#1826);
#1530=AXIS2_PLACEMENT_3D('',#2304,#1831,#1832);
#1531=AXIS2_PLACEMENT_3D('',#2307,#1835,#1836);
#1532=AXIS2_PLACEMENT_3D('',#2308,#1837,#1838);
#1533=AXIS2_PLACEMENT_3D('',#2309,#1839,#1840);
#1534=AXIS2_PLACEMENT_3D('',#2310,#1841,#1842);
#1535=AXIS2_PLACEMENT_3D('',#2311,#1843,#1844);
#1536=AXIS2_PLACEMENT_3D('',#2312,#1845,#1846);
#1537=AXIS2_PLACEMENT_3D('',#2313,#1847,#1848);
#1538=AXIS2_PLACEMENT_3D('',#2314,#1849,#1850);
#1539=AXIS2_PLACEMENT_3D('',#2315,#1851,#1852);
#1540=AXIS2_PLACEMENT_3D('',#2316,#1853,#1854);
#1541=AXIS2_PLACEMENT_3D('',#2317,#1855,#1856);
#1542=AXIS2_PLACEMENT_3D('',#2318,#1857,#1858);
#1543=AXIS2_PLACEMENT_3D('',#2319,#1859,#1860);
#1544=AXIS2_PLACEMENT_3D('',#2320,#1861,#1862);
#1545=AXIS2_PLACEMENT_3D('',#2321,#1863,#1864);
#1546=AXIS2_PLACEMENT_3D('',#2322,#1865,#1866);
#1547=AXIS2_PLACEMENT_3D('',#2324,#1867,#1868);
#1548=AXIS2_PLACEMENT_3D('',#2327,#1870,#1871);
#1549=AXIS2_PLACEMENT_3D('',#2328,#1872,#1873);
#1550=AXIS2_PLACEMENT_3D('',#2329,#1874,#1875);
#1551=AXIS2_PLACEMENT_3D('',#2330,#1876,#1877);
#1552=AXIS2_PLACEMENT_3D('',#2331,#1878,#1879);
#1553=AXIS2_PLACEMENT_3D('',#2334,#1880,#1881);
#1554=AXIS2_PLACEMENT_3D('',#2335,#1882,#1883);
#1555=AXIS2_PLACEMENT_3D('',#2337,#1884,#1885);
#1556=AXIS2_PLACEMENT_3D('',#2338,#1886,#1887);
#1557=AXIS2_PLACEMENT_3D('',#2339,#1888,#1889);
#1558=AXIS2_PLACEMENT_3D('',#2342,#1890,#1891);
#1559=AXIS2_PLACEMENT_3D('',#2344,#1892,#1893);
#1560=AXIS2_PLACEMENT_3D('',#2346,#1894,#1895);
#1561=AXIS2_PLACEMENT_3D('',#2349,#1897,#1898);
#1562=AXIS2_PLACEMENT_3D('',#2351,#1899,#1900);
#1563=AXIS2_PLACEMENT_3D('',#2353,#1901,#1902);
#1564=AXIS2_PLACEMENT_3D('',#2354,#1903,#1904);
#1565=AXIS2_PLACEMENT_3D('',#2355,#1905,#1906);
#1566=AXIS2_PLACEMENT_3D('',#2357,#1907,#1908);
#1567=AXIS2_PLACEMENT_3D('',#2360,#1910,#1911);
#1568=AXIS2_PLACEMENT_3D('',#2361,#1912,#1913);
#1569=AXIS2_PLACEMENT_3D('',#2363,#1915,#1916);
#1570=AXIS2_PLACEMENT_3D('',#2364,#1917,#1918);
#1571=AXIS2_PLACEMENT_3D('',#2365,#1919,#1920);
#1572=AXIS2_PLACEMENT_3D('',#2369,#1923,#1924);
#1573=AXIS2_PLACEMENT_3D('',#2373,#1927,#1928);
#1574=AXIS2_PLACEMENT_3D('',#2377,#1931,#1932);
#1575=AXIS2_PLACEMENT_3D('',#2381,#1935,#1936);
#1576=AXIS2_PLACEMENT_3D('',#2385,#1939,#1940);
#1577=AXIS2_PLACEMENT_3D('',#2389,#1943,#1944);
#1578=AXIS2_PLACEMENT_3D('',#2392,#1945,#1946);
#1579=AXIS2_PLACEMENT_3D('',#2394,#1947,#1948);
#1580=AXIS2_PLACEMENT_3D('',#2396,#1949,#1950);
#1581=AXIS2_PLACEMENT_3D('',#2398,#1951,#1952);
#1582=AXIS2_PLACEMENT_3D('',#2400,#1953,#1954);
#1583=AXIS2_PLACEMENT_3D('',#2401,#1955,#1956);
#1584=AXIS2_PLACEMENT_3D('',#2402,#1957,#1958);
#1585=AXIS2_PLACEMENT_3D('',#2410,#1959,#1960);
#1586=AXIS2_PLACEMENT_3D('',#2418,#1961,#1962);
#1587=AXIS2_PLACEMENT_3D('',#2426,#1963,#1964);
#1588=AXIS2_PLACEMENT_3D('',#2434,#1965,#1966);
#1589=AXIS2_PLACEMENT_3D('',#2442,#1967,#1968);
#1590=AXIS2_PLACEMENT_3D('',#2450,#1969,#1970);
#1591=AXIS2_PLACEMENT_3D('',#2453,#1973,#1974);
#1592=AXIS2_PLACEMENT_3D('',#2455,#1976,#1977);
#1593=AXIS2_PLACEMENT_3D('',#2457,#1979,#1980);
#1594=AXIS2_PLACEMENT_3D('',#2459,#1982,#1983);
#1595=AXIS2_PLACEMENT_3D('',#2461,#1985,#1986);
#1596=AXIS2_PLACEMENT_3D('',#2462,#1987,#1988);
#1597=AXIS2_PLACEMENT_3D('',#2463,#1989,#1990);
#1598=AXIS2_PLACEMENT_3D('',#2464,#1991,#1992);
#1599=AXIS2_PLACEMENT_3D('',#2465,#1993,#1994);
#1600=DIRECTION('axis',(0.,0.,1.));
#1601=DIRECTION('refdir',(1.,0.,0.));
#1602=DIRECTION('axis',(0.,0.,1.));
#1603=DIRECTION('refdir',(1.,0.,0.));
#1604=DIRECTION('center_axis',(-1.,0.,0.));
#1605=DIRECTION('ref_axis',(0.,0.,1.));
#1606=DIRECTION('',(0.,0.,1.));
#1607=DIRECTION('',(0.,1.,0.));
#1608=DIRECTION('',(0.,0.,1.));
#1609=DIRECTION('',(0.,-1.,0.));
#1610=DIRECTION('center_axis',(1.,0.,0.));
#1611=DIRECTION('ref_axis',(0.,0.,-1.));
#1612=DIRECTION('',(0.,0.,1.));
#1613=DIRECTION('',(0.,-1.,0.));
#1614=DIRECTION('',(0.,0.,1.));
#1615=DIRECTION('',(0.,1.,0.));
#1616=DIRECTION('center_axis',(-1.,0.,0.));
#1617=DIRECTION('ref_axis',(0.,0.,1.));
#1618=DIRECTION('',(0.,-1.,0.));
#1619=DIRECTION('',(0.,0.,1.));
#1620=DIRECTION('',(0.,-1.,0.));
#1621=DIRECTION('',(0.,0.,1.));
#1622=DIRECTION('center_axis',(0.,1.,0.));
#1623=DIRECTION('ref_axis',(0.,0.,1.));
#1624=DIRECTION('',(-1.,0.,0.));
#1625=DIRECTION('',(0.,0.,1.));
#1626=DIRECTION('',(-1.,0.,0.));
#1627=DIRECTION('center_axis',(-1.,0.,0.));
#1628=DIRECTION('ref_axis',(0.,0.,1.));
#1629=DIRECTION('',(0.,-1.,0.));
#1630=DIRECTION('',(0.,0.,1.));
#1631=DIRECTION('',(0.,-1.,0.));
#1632=DIRECTION('center_axis',(0.,-1.,0.));
#1633=DIRECTION('ref_axis',(0.,0.,-1.));
#1634=DIRECTION('',(1.,0.,0.));
#1635=DIRECTION('',(1.,0.,0.));
#1636=DIRECTION('',(0.,0.,1.));
#1637=DIRECTION('',(1.,0.,0.));
#1638=DIRECTION('center_axis',(0.,1.,0.));
#1639=DIRECTION('ref_axis',(0.,0.,1.));
#1640=DIRECTION('',(-1.,0.,0.));
#1641=DIRECTION('',(0.,0.,1.));
#1642=DIRECTION('',(-1.,0.,0.));
#1643=DIRECTION('',(0.,0.,-1.));
#1644=DIRECTION('',(1.,0.,0.));
#1645=DIRECTION('center_axis',(0.707106781186548,0.707106781186548,0.));
#1646=DIRECTION('ref_axis',(-0.707106781186548,0.707106781186548,0.));
#1647=DIRECTION('',(-0.707106781186547,0.707106781186547,0.));
#1648=DIRECTION('',(0.,0.,1.));
#1649=DIRECTION('',(-0.707106781186547,0.707106781186547,0.));
#1650=DIRECTION('center_axis',(1.,0.,0.));
#1651=DIRECTION('ref_axis',(0.,0.,-1.));
#1652=DIRECTION('',(0.,1.,0.));
#1653=DIRECTION('',(0.,0.,1.));
#1654=DIRECTION('',(0.,1.,0.));
#1655=DIRECTION('center_axis',(0.,1.,0.));
#1656=DIRECTION('ref_axis',(0.,0.,1.));
#1657=DIRECTION('',(-1.,0.,0.));
#1658=DIRECTION('',(0.,0.,1.));
#1659=DIRECTION('',(-1.,0.,0.));
#1660=DIRECTION('center_axis',(-1.,0.,0.));
#1661=DIRECTION('ref_axis',(0.,0.,1.));
#1662=DIRECTION('',(0.,-1.,0.));
#1663=DIRECTION('',(0.,0.,1.));
#1664=DIRECTION('',(0.,-1.,0.));
#1665=DIRECTION('center_axis',(-0.707106781186548,0.707106781186548,0.));
#1666=DIRECTION('ref_axis',(-0.707106781186548,-0.707106781186548,0.));
#1667=DIRECTION('',(-0.707106781186547,-0.707106781186547,0.));
#1668=DIRECTION('',(0.,0.,1.));
#1669=DIRECTION('',(-0.707106781186547,-0.707106781186547,0.));
#1670=DIRECTION('center_axis',(0.,1.,0.));
#1671=DIRECTION('ref_axis',(0.,0.,1.));
#1672=DIRECTION('',(-1.,0.,0.));
#1673=DIRECTION('',(-1.,0.,0.));
#1674=DIRECTION('',(0.,0.,1.));
#1675=DIRECTION('',(-1.,0.,0.));
#1676=DIRECTION('center_axis',(0.,-1.,0.));
#1677=DIRECTION('ref_axis',(0.,0.,-1.));
#1678=DIRECTION('',(1.,0.,0.));
#1679=DIRECTION('',(0.,0.,1.));
#1680=DIRECTION('',(1.,0.,0.));
#1681=DIRECTION('',(0.,0.,-1.));
#1682=DIRECTION('',(-1.,0.,0.));
#1683=DIRECTION('center_axis',(0.999999999999972,-2.35372237672442E-7,0.));
#1684=DIRECTION('ref_axis',(2.35372237672442E-7,0.999999999999972,0.));
#1685=DIRECTION('',(2.35372237672442E-7,0.999999999999972,0.));
#1686=DIRECTION('',(0.,0.,1.));
#1687=DIRECTION('',(2.35372237672442E-7,0.999999999999972,0.));
#1688=DIRECTION('center_axis',(0.,1.,0.));
#1689=DIRECTION('ref_axis',(0.,0.,1.));
#1690=DIRECTION('',(-1.,0.,0.));
#1691=DIRECTION('',(0.,0.,1.));
#1692=DIRECTION('',(-1.,0.,0.));
#1693=DIRECTION('center_axis',(1.,0.,0.));
#1694=DIRECTION('ref_axis',(0.,0.,-1.));
#1695=DIRECTION('',(0.,1.,0.));
#1696=DIRECTION('',(0.,0.,1.));
#1697=DIRECTION('',(0.,1.,0.));
#1698=DIRECTION('center_axis',(0.,-1.,0.));
#1699=DIRECTION('ref_axis',(0.,0.,-1.));
#1700=DIRECTION('',(1.,0.,0.));
#1701=DIRECTION('',(0.,0.,1.));
#1702=DIRECTION('',(1.,0.,0.));
#1703=DIRECTION('center_axis',(-0.866025403784439,0.5,0.));
#1704=DIRECTION('ref_axis',(-0.5,-0.866025403784439,0.));
#1705=DIRECTION('',(-0.5,-0.866025403784439,0.));
#1706=DIRECTION('',(0.,0.,1.));
#1707=DIRECTION('',(-0.5,-0.866025403784439,0.));
#1708=DIRECTION('center_axis',(0.,-1.,0.));
#1709=DIRECTION('ref_axis',(0.,0.,-1.));
#1710=DIRECTION('',(1.,0.,0.));
#1711=DIRECTION('',(0.,0.,1.));
#1712=DIRECTION('',(1.,0.,0.));
#1713=DIRECTION('center_axis',(0.866025403784439,0.5,0.));
#1714=DIRECTION('ref_axis',(-0.5,0.866025403784439,0.));
#1715=DIRECTION('',(-0.5,0.866025403784439,0.));
#1716=DIRECTION('',(0.,0.,1.));
#1717=DIRECTION('',(-0.5,0.866025403784439,0.));
#1718=DIRECTION('center_axis',(0.,-1.,0.));
#1719=DIRECTION('ref_axis',(0.,0.,-1.));
#1720=DIRECTION('',(1.,0.,0.));
#1721=DIRECTION('',(1.,0.,0.));
#1722=DIRECTION('center_axis',(0.,0.,-1.));
#1723=DIRECTION('ref_axis',(-1.,0.,0.));
#1724=DIRECTION('',(0.,-1.,0.));
#1725=DIRECTION('',(0.,1.,0.));
#1726=DIRECTION('center_axis',(0.,0.,-1.));
#1727=DIRECTION('ref_axis',(-1.,0.,0.));
#1728=DIRECTION('center_axis',(0.,0.,-1.));
#1729=DIRECTION('ref_axis',(-1.,0.,0.));
#1730=DIRECTION('',(0.,-1.,0.));
#1731=DIRECTION('center_axis',(1.,0.,0.));
#1732=DIRECTION('ref_axis',(0.,0.,-1.));
#1733=DIRECTION('center_axis',(0.,0.,-1.));
#1734=DIRECTION('ref_axis',(-1.,0.,0.));
#1735=DIRECTION('',(0.,1.,0.));
#1736=DIRECTION('center_axis',(1.,0.,0.));
#1737=DIRECTION('ref_axis',(0.,0.,-1.));
#1738=DIRECTION('axis',(0.,0.,1.));
#1739=DIRECTION('refdir',(1.,0.,0.));
#1740=DIRECTION('center_axis',(0.,1.,0.));
#1741=DIRECTION('ref_axis',(0.,0.,1.));
#1742=DIRECTION('',(0.,1.,0.));
#1743=DIRECTION('center_axis',(0.,1.,0.));
#1744=DIRECTION('ref_axis',(0.,0.,1.));
#1745=DIRECTION('center_axis',(0.,1.,0.));
#1746=DIRECTION('ref_axis',(0.,0.,1.));
#1747=DIRECTION('',(-1.,0.,0.));
#1748=DIRECTION('',(0.,0.,1.));
#1749=DIRECTION('',(-1.,0.,0.));
#1750=DIRECTION('',(0.,0.,1.));
#1751=DIRECTION('center_axis',(-1.,-2.47817639425258E-16,0.));
#1752=DIRECTION('ref_axis',(2.47817639425258E-16,-1.,0.));
#1753=DIRECTION('',(2.47817639425258E-16,-1.,0.));
#1754=DIRECTION('',(0.,0.,1.));
#1755=DIRECTION('',(2.47817639425258E-16,-1.,0.));
#1756=DIRECTION('center_axis',(0.,0.,1.));
#1757=DIRECTION('ref_axis',(1.,0.,0.));
#1758=DIRECTION('center_axis',(0.,0.,-1.));
#1759=DIRECTION('ref_axis',(1.,0.,0.));
#1760=DIRECTION('',(0.,0.,1.));
#1761=DIRECTION('center_axis',(0.,0.,-1.));
#1762=DIRECTION('ref_axis',(1.,0.,0.));
#1763=DIRECTION('center_axis',(1.,0.,0.));
#1764=DIRECTION('ref_axis',(0.,0.,-1.));
#1765=DIRECTION('',(0.,1.,0.));
#1766=DIRECTION('',(0.,0.,1.));
#1767=DIRECTION('',(0.,1.,0.));
#1768=DIRECTION('center_axis',(0.,1.,0.));
#1769=DIRECTION('ref_axis',(0.,0.,1.));
#1770=DIRECTION('',(-1.,0.,0.));
#1771=DIRECTION('',(0.,0.,1.));
#1772=DIRECTION('',(-1.,0.,0.));
#1773=DIRECTION('center_axis',(1.,0.,0.));
#1774=DIRECTION('ref_axis',(0.,0.,-1.));
#1775=DIRECTION('',(0.,1.,0.));
#1776=DIRECTION('',(0.,0.,1.));
#1777=DIRECTION('',(0.,1.,0.));
#1778=DIRECTION('center_axis',(0.,-1.,0.));
#1779=DIRECTION('ref_axis',(0.,0.,-1.));
#1780=DIRECTION('',(1.,0.,0.));
#1781=DIRECTION('',(0.,0.,-1.));
#1782=DIRECTION('',(1.,0.,0.));
#1783=DIRECTION('center_axis',(-1.,-9.91270557701033E-17,0.));
#1784=DIRECTION('ref_axis',(9.91270557701033E-17,-1.,0.));
#1785=DIRECTION('',(9.91270557701033E-17,-1.,0.));
#1786=DIRECTION('',(0.,0.,1.));
#1787=DIRECTION('',(9.91270557701033E-17,-1.,0.));
#1788=DIRECTION('',(0.,0.,1.));
#1789=DIRECTION('center_axis',(0.,0.,1.));
#1790=DIRECTION('ref_axis',(1.,0.,0.));
#1791=DIRECTION('center_axis',(0.,0.,1.));
#1792=DIRECTION('ref_axis',(1.,0.,0.));
#1793=DIRECTION('',(0.,0.,-1.));
#1794=DIRECTION('center_axis',(0.,0.,1.));
#1795=DIRECTION('ref_axis',(1.,0.,0.));
#1796=DIRECTION('center_axis',(-1.,0.,0.));
#1797=DIRECTION('ref_axis',(0.,0.,1.));
#1798=DIRECTION('',(0.,-1.,0.));
#1799=DIRECTION('',(0.,0.,1.));
#1800=DIRECTION('',(0.,-1.,0.));
#1801=DIRECTION('',(0.,0.,1.));
#1802=DIRECTION('center_axis',(0.,1.,0.));
#1803=DIRECTION('ref_axis',(0.,0.,1.));
#1804=DIRECTION('',(-1.,0.,0.));
#1805=DIRECTION('',(0.,0.,1.));
#1806=DIRECTION('',(-1.,0.,0.));
#1807=DIRECTION('center_axis',(1.,0.,0.));
#1808=DIRECTION('ref_axis',(0.,0.,-1.));
#1809=DIRECTION('',(0.,1.,0.));
#1810=DIRECTION('',(0.,0.,-1.));
#1811=DIRECTION('',(0.,1.,0.));
#1812=DIRECTION('center_axis',(0.,0.,1.));
#1813=DIRECTION('ref_axis',(1.,0.,0.));
#1814=DIRECTION('center_axis',(0.,0.,1.));
#1815=DIRECTION('ref_axis',(1.,0.,0.));
#1816=DIRECTION('',(0.,0.,1.));
#1817=DIRECTION('center_axis',(0.,0.,1.));
#1818=DIRECTION('ref_axis',(1.,0.,0.));
#1819=DIRECTION('',(0.,0.,1.));
#1820=DIRECTION('center_axis',(1.,0.,0.));
#1821=DIRECTION('ref_axis',(0.,0.,-1.));
#1822=DIRECTION('',(0.,1.,0.));
#1823=DIRECTION('',(0.,0.,-1.));
#1824=DIRECTION('',(0.,1.,0.));
#1825=DIRECTION('center_axis',(0.,-1.,0.));
#1826=DIRECTION('ref_axis',(0.,0.,-1.));
#1827=DIRECTION('',(1.,0.,0.));
#1828=DIRECTION('',(0.,0.,1.));
#1829=DIRECTION('',(1.,0.,0.));
#1830=DIRECTION('',(0.,0.,1.));
#1831=DIRECTION('center_axis',(-1.,0.,0.));
#1832=DIRECTION('ref_axis',(0.,0.,1.));
#1833=DIRECTION('',(0.,-1.,0.));
#1834=DIRECTION('',(0.,-1.,0.));
#1835=DIRECTION('center_axis',(0.,0.,1.));
#1836=DIRECTION('ref_axis',(1.,0.,0.));
#1837=DIRECTION('center_axis',(0.,0.,-1.));
#1838=DIRECTION('ref_axis',(1.,0.,0.));
#1839=DIRECTION('center_axis',(0.,0.,-1.));
#1840=DIRECTION('ref_axis',(1.,0.,0.));
#1841=DIRECTION('center_axis',(0.,0.,1.));
#1842=DIRECTION('ref_axis',(1.,0.,0.));
#1843=DIRECTION('center_axis',(0.,0.,1.));
#1844=DIRECTION('ref_axis',(1.,0.,0.));
#1845=DIRECTION('center_axis',(0.,0.,1.));
#1846=DIRECTION('ref_axis',(1.,0.,0.));
#1847=DIRECTION('center_axis',(0.,0.,1.));
#1848=DIRECTION('ref_axis',(1.,0.,0.));
#1849=DIRECTION('center_axis',(0.,0.,-1.));
#1850=DIRECTION('ref_axis',(1.,0.,0.));
#1851=DIRECTION('center_axis',(0.,0.,-1.));
#1852=DIRECTION('ref_axis',(1.,0.,0.));
#1853=DIRECTION('center_axis',(0.,0.,1.));
#1854=DIRECTION('ref_axis',(1.,0.,0.));
#1855=DIRECTION('center_axis',(0.,0.,1.));
#1856=DIRECTION('ref_axis',(1.,0.,0.));
#1857=DIRECTION('center_axis',(0.,0.,1.));
#1858=DIRECTION('ref_axis',(1.,0.,0.));
#1859=DIRECTION('center_axis',(0.,0.,1.));
#1860=DIRECTION('ref_axis',(1.,0.,0.));
#1861=DIRECTION('center_axis',(0.,0.,1.));
#1862=DIRECTION('ref_axis',(1.,0.,0.));
#1863=DIRECTION('axis',(0.,0.,1.));
#1864=DIRECTION('refdir',(1.,0.,0.));
#1865=DIRECTION('center_axis',(0.,0.,1.));
#1866=DIRECTION('ref_axis',(1.,0.,0.));
#1867=DIRECTION('center_axis',(0.,0.,1.));
#1868=DIRECTION('ref_axis',(1.,0.,0.));
#1869=DIRECTION('',(0.,0.,-1.));
#1870=DIRECTION('center_axis',(0.,0.,1.));
#1871=DIRECTION('ref_axis',(1.,0.,0.));
#1872=DIRECTION('center_axis',(0.,0.,1.));
#1873=DIRECTION('ref_axis',(1.,0.,0.));
#1874=DIRECTION('center_axis',(0.,0.,1.));
#1875=DIRECTION('ref_axis',(1.,0.,0.));
#1876=DIRECTION('axis',(0.,0.,1.));
#1877=DIRECTION('refdir',(1.,0.,0.));
#1878=DIRECTION('center_axis',(1.,0.,0.));
#1879=DIRECTION('ref_axis',(0.,0.,-1.));
#1880=DIRECTION('center_axis',(1.,0.,0.));
#1881=DIRECTION('ref_axis',(0.,0.,-1.));
#1882=DIRECTION('center_axis',(1.,0.,0.));
#1883=DIRECTION('ref_axis',(0.,0.,-1.));
#1884=DIRECTION('center_axis',(0.,1.,1.22464683884653E-16));
#1885=DIRECTION('ref_axis',(0.,-1.22464683884653E-16,1.));
#1886=DIRECTION('center_axis',(-1.,0.,0.));
#1887=DIRECTION('ref_axis',(0.,0.,-1.));
#1888=DIRECTION('center_axis',(-1.,0.,0.));
#1889=DIRECTION('ref_axis',(0.,0.,1.));
#1890=DIRECTION('center_axis',(-1.,0.,0.));
#1891=DIRECTION('ref_axis',(0.,0.,1.));
#1892=DIRECTION('center_axis',(-1.,0.,0.));
#1893=DIRECTION('ref_axis',(0.,0.,1.));
#1894=DIRECTION('center_axis',(-1.,0.,0.));
#1895=DIRECTION('ref_axis',(0.,0.,1.));
#1896=DIRECTION('',(1.,0.,0.));
#1897=DIRECTION('center_axis',(1.,0.,0.));
#1898=DIRECTION('ref_axis',(0.,0.,-1.));
#1899=DIRECTION('center_axis',(-1.,0.,0.));
#1900=DIRECTION('ref_axis',(0.,0.,1.));
#1901=DIRECTION('center_axis',(-1.,0.,0.));
#1902=DIRECTION('ref_axis',(0.,0.,1.));
#1903=DIRECTION('center_axis',(-1.,0.,0.));
#1904=DIRECTION('ref_axis',(0.,0.,1.));
#1905=DIRECTION('center_axis',(-1.,0.,0.));
#1906=DIRECTION('ref_axis',(0.,0.,1.));
#1907=DIRECTION('center_axis',(-1.,0.,0.));
#1908=DIRECTION('ref_axis',(0.,0.,1.));
#1909=DIRECTION('',(0.707106781186547,8.65956056235494E-17,0.707106781186548));
#1910=DIRECTION('center_axis',(-1.,0.,0.));
#1911=DIRECTION('ref_axis',(0.,0.,1.));
#1912=DIRECTION('center_axis',(-1.,0.,0.));
#1913=DIRECTION('ref_axis',(0.,0.,1.));
#1914=DIRECTION('',(1.,0.,0.));
#1915=DIRECTION('center_axis',(1.,0.,0.));
#1916=DIRECTION('ref_axis',(0.,0.,-1.));
#1917=DIRECTION('center_axis',(-1.,0.,0.));
#1918=DIRECTION('ref_axis',(0.,0.,1.));
#1919=DIRECTION('center_axis',(1.,0.,0.));
#1920=DIRECTION('ref_axis',(0.,0.,-1.));
#1921=DIRECTION('',(0.,0.500000000000001,0.866025403784438));
#1922=DIRECTION('',(0.,1.,0.));
#1923=DIRECTION('center_axis',(1.,0.,0.));
#1924=DIRECTION('ref_axis',(0.,0.,-1.));
#1925=DIRECTION('',(0.,0.500000000000001,0.866025403784438));
#1926=DIRECTION('',(0.,-0.500000000000001,0.866025403784438));
#1927=DIRECTION('center_axis',(1.,0.,0.));
#1928=DIRECTION('ref_axis',(0.,0.,-1.));
#1929=DIRECTION('',(0.,-0.500000000000001,0.866025403784438));
#1930=DIRECTION('',(0.,-1.,-1.66923844304129E-16));
#1931=DIRECTION('center_axis',(1.,0.,0.));
#1932=DIRECTION('ref_axis',(0.,0.,-1.));
#1933=DIRECTION('',(0.,-1.,-1.66923844304129E-16));
#1934=DIRECTION('',(0.,-0.500000000000002,-0.866025403784438));
#1935=DIRECTION('center_axis',(1.,0.,0.));
#1936=DIRECTION('ref_axis',(0.,0.,-1.));
#1937=DIRECTION('',(0.,-0.500000000000002,-0.866025403784438));
#1938=DIRECTION('',(0.,0.5,-0.866025403784439));
#1939=DIRECTION('center_axis',(1.,0.,0.));
#1940=DIRECTION('ref_axis',(0.,0.,-1.));
#1941=DIRECTION('',(0.,0.5,-0.866025403784439));
#1942=DIRECTION('',(0.,1.,0.));
#1943=DIRECTION('center_axis',(1.,0.,0.));
#1944=DIRECTION('ref_axis',(0.,0.,-1.));
#1945=DIRECTION('center_axis',(1.,0.,0.));
#1946=DIRECTION('ref_axis',(0.,0.,-1.));
#1947=DIRECTION('center_axis',(1.,0.,0.));
#1948=DIRECTION('ref_axis',(0.,0.,-1.));
#1949=DIRECTION('center_axis',(1.,0.,0.));
#1950=DIRECTION('ref_axis',(0.,0.,-1.));
#1951=DIRECTION('center_axis',(1.,0.,0.));
#1952=DIRECTION('ref_axis',(0.,0.,-1.));
#1953=DIRECTION('center_axis',(-1.,0.,0.));
#1954=DIRECTION('ref_axis',(0.,0.,1.));
#1955=DIRECTION('center_axis',(1.,0.,0.));
#1956=DIRECTION('ref_axis',(0.,0.,-1.));
#1957=DIRECTION('center_axis',(1.,0.,0.));
#1958=DIRECTION('ref_axis',(0.,0.,-1.));
#1959=DIRECTION('center_axis',(1.,0.,0.));
#1960=DIRECTION('ref_axis',(0.,0.,-1.));
#1961=DIRECTION('center_axis',(1.,0.,0.));
#1962=DIRECTION('ref_axis',(0.,0.,-1.));
#1963=DIRECTION('center_axis',(1.,0.,0.));
#1964=DIRECTION('ref_axis',(0.,0.,-1.));
#1965=DIRECTION('center_axis',(1.,0.,0.));
#1966=DIRECTION('ref_axis',(0.,0.,-1.));
#1967=DIRECTION('center_axis',(1.,0.,0.));
#1968=DIRECTION('ref_axis',(0.,0.,-1.));
#1969=DIRECTION('center_axis',(0.,0.,1.));
#1970=DIRECTION('ref_axis',(1.,0.,0.));
#1971=DIRECTION('',(-1.,0.,0.));
#1972=DIRECTION('',(-1.,0.,0.));
#1973=DIRECTION('center_axis',(0.,0.866025403784439,0.5));
#1974=DIRECTION('ref_axis',(0.,-0.5,0.866025403784439));
#1975=DIRECTION('',(-1.,0.,0.));
#1976=DIRECTION('center_axis',(0.,0.866025403784438,-0.500000000000002));
#1977=DIRECTION('ref_axis',(0.,0.500000000000002,0.866025403784437));
#1978=DIRECTION('',(-1.,0.,0.));
#1979=DIRECTION('center_axis',(0.,1.66923844304129E-16,-1.));
#1980=DIRECTION('ref_axis',(0.,1.,1.66923844304129E-16));
#1981=DIRECTION('',(-1.,0.,0.));
#1982=DIRECTION('center_axis',(0.,-0.866025403784438,-0.500000000000001));
#1983=DIRECTION('ref_axis',(0.,0.500000000000001,-0.866025403784438));
#1984=DIRECTION('',(-1.,0.,0.));
#1985=DIRECTION('center_axis',(0.,-0.866025403784438,0.500000000000001));
#1986=DIRECTION('ref_axis',(0.,-0.500000000000001,-0.866025403784438));
#1987=DIRECTION('',(0.,0.,1.));
#1988=DIRECTION('',(1.,0.,0.));
#1989=DIRECTION('',(0.,0.,1.));
#1990=DIRECTION('',(1.,0.,0.));
#1991=DIRECTION('',(0.,0.,1.));
#1992=DIRECTION('',(0.998621318874715,-0.0524924898335409,0.));
#1993=DIRECTION('',(0.205106371564066,0.,-0.978739687733068));
#1994=DIRECTION('',(0.,-1.,0.));
#1995=CARTESIAN_POINT('',(0.,0.,0.));
#1996=CARTESIAN_POINT('',(0.,0.,0.));
#1997=CARTESIAN_POINT('Origin',(-36.9999998586142,28.9943965601659,-119.188676592855));
#1998=CARTESIAN_POINT('',(-36.9999998586142,52.994396560166,-89.1886765928545));
#1999=CARTESIAN_POINT('',(-36.9999998586142,52.994396560166,40.8113234071455));
#2000=CARTESIAN_POINT('',(-36.9999998586142,52.994396560166,-119.188676592855));
#2001=CARTESIAN_POINT('',(-36.9999998586142,28.9943965601659,-89.1886765928545));
#2002=CARTESIAN_POINT('',(-36.9999998586142,52.994396560166,-89.1886765928545));
#2003=CARTESIAN_POINT('',(-36.9999998586142,28.9943965601659,40.8113234071455));
#2004=CARTESIAN_POINT('',(-36.9999998586142,28.9943965601659,-119.188676592855));
#2005=CARTESIAN_POINT('',(-36.9999998586142,28.9943965601659,40.8113234071455));
#2006=CARTESIAN_POINT('Origin',(37.0000001413876,28.9943965606416,-119.188676592855));
#2007=CARTESIAN_POINT('',(37.0000001413876,28.9943965606416,-89.1886765928545));
#2008=CARTESIAN_POINT('',(37.0000001413876,28.9943965606416,40.8113234071455));
#2009=CARTESIAN_POINT('',(37.0000001413876,28.9943965606416,-119.188676592855));
#2010=CARTESIAN_POINT('',(37.0000001413876,52.9943965606364,-89.1886765928545));
#2011=CARTESIAN_POINT('',(37.0000001413876,52.9943965606364,-89.1886765928545));
#2012=CARTESIAN_POINT('',(37.0000001413876,52.9943965606364,40.8113234071455));
#2013=CARTESIAN_POINT('',(37.0000001413876,52.9943965606364,-119.188676592855));
#2014=CARTESIAN_POINT('',(37.0000001413876,28.9943965606416,40.8113234071455));
#2015=CARTESIAN_POINT('Origin',(-49.9999998586142,-15.0056034398341,-119.188676592855));
#2016=CARTESIAN_POINT('',(-49.9999998586142,8.99439656016592,40.8113234071455));
#2017=CARTESIAN_POINT('',(-49.9999998586142,-15.0056034398341,40.8113234071455));
#2018=CARTESIAN_POINT('',(-49.9999998586142,-15.0056034398341,40.8113234071455));
#2019=CARTESIAN_POINT('',(-49.9999998586142,8.99439656016592,-119.188676592855));
#2020=CARTESIAN_POINT('',(-49.9999998586142,8.99439656016592,-119.188676592855));
#2021=CARTESIAN_POINT('',(-49.9999998586142,-15.0056034398341,-119.188676592855));
#2022=CARTESIAN_POINT('',(-49.9999998586142,-15.0056034398341,-119.188676592855));
#2023=CARTESIAN_POINT('',(-49.9999998586142,-15.0056034398341,-119.188676592855));
#2024=CARTESIAN_POINT('Origin',(-49.9999998586142,8.99439656016592,-119.188676592855));
#2025=CARTESIAN_POINT('',(-25.9999998586142,8.99439656016592,40.8113234071455));
#2026=CARTESIAN_POINT('',(-49.9999998586142,8.99439656016592,40.8113234071455));
#2027=CARTESIAN_POINT('',(-25.9999998586142,8.99439656016592,-119.188676592855));
#2028=CARTESIAN_POINT('',(-25.9999998586142,8.99439656016592,-119.188676592855));
#2029=CARTESIAN_POINT('',(-49.9999998586142,8.99439656016592,-119.188676592855));
#2030=CARTESIAN_POINT('Origin',(-25.9999998586142,8.99439656016592,-119.188676592855));
#2031=CARTESIAN_POINT('',(-25.9999998586142,28.9943965601659,40.8113234071455));
#2032=CARTESIAN_POINT('',(-25.9999998586142,8.99439656016592,40.8113234071455));
#2033=CARTESIAN_POINT('',(-25.9999998586142,28.9943965601659,-119.188676592855));
#2034=CARTESIAN_POINT('',(-25.9999998586142,28.9943965601659,-119.188676592855));
#2035=CARTESIAN_POINT('',(-25.9999998586142,8.99439656016592,-119.188676592855));
#2036=CARTESIAN_POINT('Origin',(-25.9999998586142,28.9943965601659,-119.188676592855));
#2037=CARTESIAN_POINT('',(-25.9999998586142,28.9943965601659,40.8113234071455));
#2038=CARTESIAN_POINT('',(-48.9999998586142,28.9943965601659,-89.1886765928545));
#2039=CARTESIAN_POINT('',(-48.9999998586142,28.9943965601659,-89.1886765928545));
#2040=CARTESIAN_POINT('',(-48.9999998586142,28.9943965601659,-119.188676592855));
#2041=CARTESIAN_POINT('',(-48.9999998586142,28.9943965601659,-89.1886765928545));
#2042=CARTESIAN_POINT('',(-25.9999998586142,28.9943965601659,-119.188676592855));
#2043=CARTESIAN_POINT('Origin',(-36.9999998586142,52.994396560166,-119.188676592855));
#2044=CARTESIAN_POINT('',(-24.9999998586142,52.994396560166,40.8113234071455));
#2045=CARTESIAN_POINT('',(-36.9999998586142,52.994396560166,40.8113234071455));
#2046=CARTESIAN_POINT('',(-24.9999998586142,52.994396560166,-119.188676592855));
#2047=CARTESIAN_POINT('',(-24.9999998586142,52.994396560166,-119.188676592855));
#2048=CARTESIAN_POINT('',(-48.9999998586142,52.994396560166,-119.188676592855));
#2049=CARTESIAN_POINT('',(-36.9999998586142,52.994396560166,-119.188676592855));
#2050=CARTESIAN_POINT('',(-48.9999998586142,52.994396560166,-89.1886765928545));
#2051=CARTESIAN_POINT('',(-48.9999998586142,52.994396560166,-119.188676592855));
#2052=CARTESIAN_POINT('',(-48.9999998586142,52.994396560166,-89.1886765928545));
#2053=CARTESIAN_POINT('Origin',(-24.9999998586142,52.994396560166,-119.188676592855));
#2054=CARTESIAN_POINT('',(-2.99999985861422,30.994396560166,40.8113234071455));
#2055=CARTESIAN_POINT('',(-24.9999998586142,52.994396560166,40.8113234071455));
#2056=CARTESIAN_POINT('',(-2.99999985861422,30.994396560166,-119.188676592855));
#2057=CARTESIAN_POINT('',(-2.99999985861422,30.994396560166,-119.188676592855));
#2058=CARTESIAN_POINT('',(-24.9999998586142,52.994396560166,-119.188676592855));
#2059=CARTESIAN_POINT('Origin',(-2.99999985861422,30.994396560166,-119.188676592855));
#2060=CARTESIAN_POINT('',(-2.99999985861422,26.9943965601665,40.8113234071455));
#2061=CARTESIAN_POINT('',(-2.99999985861422,30.994396560166,40.8113234071455));
#2062=CARTESIAN_POINT('',(-2.99999985861422,26.9943965601665,-119.188676592855));
#2063=CARTESIAN_POINT('',(-2.99999985861422,26.9943965601665,-119.188676592855));
#2064=CARTESIAN_POINT('',(-2.99999985861422,30.994396560166,-119.188676592855));
#2065=CARTESIAN_POINT('Origin',(-2.99999985861422,26.9943965601665,-119.188676592855));
#2066=CARTESIAN_POINT('',(3.00000014138191,26.9943965601665,40.8113234071455));
#2067=CARTESIAN_POINT('',(-2.99999985861422,26.9943965601665,40.8113234071455));
#2068=CARTESIAN_POINT('',(3.00000014138191,26.9943965601665,-119.188676592855));
#2069=CARTESIAN_POINT('',(3.00000014138191,26.9943965601665,-119.188676592855));
#2070=CARTESIAN_POINT('',(-2.99999985861422,26.9943965601665,-119.188676592855));
#2071=CARTESIAN_POINT('Origin',(3.00000014138191,30.9943965606328,-119.188676592855));
#2072=CARTESIAN_POINT('',(3.00000014138191,30.9943965606328,40.8113234071455));
#2073=CARTESIAN_POINT('',(3.00000014138191,30.9943965606328,40.8113234071455));
#2074=CARTESIAN_POINT('',(3.00000014138191,30.9943965606328,-119.188676592855));
#2075=CARTESIAN_POINT('',(3.00000014138191,30.9943965606328,-119.188676592855));
#2076=CARTESIAN_POINT('',(3.00000014138191,30.9943965606328,-119.188676592855));
#2077=CARTESIAN_POINT('Origin',(25.0000001413855,52.9943965606364,-119.188676592855));
#2078=CARTESIAN_POINT('',(25.0000001413855,52.9943965606364,40.8113234071455));
#2079=CARTESIAN_POINT('',(25.0000001413855,52.9943965606364,40.8113234071455));
#2080=CARTESIAN_POINT('',(25.0000001413855,52.9943965606364,-119.188676592855));
#2081=CARTESIAN_POINT('',(25.0000001413855,52.9943965606364,-119.188676592855));
#2082=CARTESIAN_POINT('',(25.0000001413855,52.9943965606364,-119.188676592855));
#2083=CARTESIAN_POINT('Origin',(37.0000001413876,52.9943965606364,-119.188676592855));
#2084=CARTESIAN_POINT('',(37.0000001413876,52.9943965606364,40.8113234071455));
#2085=CARTESIAN_POINT('',(49.0000001413876,52.9943965606364,-89.1886765928545));
#2086=CARTESIAN_POINT('',(49.0000001413876,52.9943965606364,-89.1886765928545));
#2087=CARTESIAN_POINT('',(49.0000001413876,52.9943965606364,-119.188676592855));
#2088=CARTESIAN_POINT('',(49.0000001413876,52.9943965606364,-119.188676592855));
#2089=CARTESIAN_POINT('',(37.0000001413876,52.9943965606364,-119.188676592855));
#2090=CARTESIAN_POINT('Origin',(26.0000001413871,28.9943965606416,-119.188676592855));
#2091=CARTESIAN_POINT('',(26.0000001413871,28.9943965606416,40.8113234071455));
#2092=CARTESIAN_POINT('',(26.0000001413871,28.9943965606416,40.8113234071455));
#2093=CARTESIAN_POINT('',(26.0000001413871,28.9943965606416,-119.188676592855));
#2094=CARTESIAN_POINT('',(26.0000001413871,28.9943965606416,-119.188676592855));
#2095=CARTESIAN_POINT('',(49.0000001413876,28.9943965606416,-119.188676592855));
#2096=CARTESIAN_POINT('',(26.0000001413871,28.9943965606416,-119.188676592855));
#2097=CARTESIAN_POINT('',(49.0000001413876,28.9943965606416,-89.1886765928545));
#2098=CARTESIAN_POINT('',(49.0000001413876,28.9943965606416,-89.1886765928545));
#2099=CARTESIAN_POINT('',(49.0000001413876,28.9943965606416,-89.1886765928545));
#2100=CARTESIAN_POINT('Origin',(25.9999954339423,8.99439656064154,-119.188676592855));
#2101=CARTESIAN_POINT('',(25.9999954339423,8.99439656064154,40.8113234071455));
#2102=CARTESIAN_POINT('',(25.9999954339423,8.99439656064154,40.8113234071455));
#2103=CARTESIAN_POINT('',(25.9999954339423,8.99439656064154,-119.188676592855));
#2104=CARTESIAN_POINT('',(25.9999954339423,8.99439656064154,-119.188676592855));
#2105=CARTESIAN_POINT('',(25.9999954339423,8.99439656064154,-119.188676592855));
#2106=CARTESIAN_POINT('Origin',(50.0000001413858,8.99439656064154,-119.188676592855));
#2107=CARTESIAN_POINT('',(50.0000001413858,8.99439656064154,40.8113234071455));
#2108=CARTESIAN_POINT('',(50.0000001413858,8.99439656064154,40.8113234071455));
#2109=CARTESIAN_POINT('',(50.0000001413858,8.99439656064154,-119.188676592855));
#2110=CARTESIAN_POINT('',(50.0000001413858,8.99439656064154,-119.188676592855));
#2111=CARTESIAN_POINT('',(50.0000001413858,8.99439656064154,-119.188676592855));
#2112=CARTESIAN_POINT('Origin',(50.0000001413858,-15.0056034398341,-119.188676592855));
#2113=CARTESIAN_POINT('',(50.0000001413858,-15.0056034398341,40.8113234071455));
#2114=CARTESIAN_POINT('',(50.0000001413858,-15.0056034398341,40.8113234071455));
#2115=CARTESIAN_POINT('',(50.0000001413858,-15.0056034398341,-119.188676592855));
#2116=CARTESIAN_POINT('',(50.0000001413858,-15.0056034398341,-119.188676592855));
#2117=CARTESIAN_POINT('',(50.0000001413858,-15.0056034398341,-119.188676592855));
#2118=CARTESIAN_POINT('Origin',(50.0000001413858,-15.0056034398341,-119.188676592855));
#2119=CARTESIAN_POINT('',(15.0000001413858,-15.0056034398341,40.8113234071455));
#2120=CARTESIAN_POINT('',(50.0000001413858,-15.0056034398341,40.8113234071455));
#2121=CARTESIAN_POINT('',(15.0000001413858,-15.0056034398341,-119.188676592855));
#2122=CARTESIAN_POINT('',(15.0000001413858,-15.0056034398341,-119.188676592855));
#2123=CARTESIAN_POINT('',(50.0000001413858,-15.0056034398341,-119.188676592855));
#2124=CARTESIAN_POINT('Origin',(15.0000001413858,-15.0056034398341,-119.188676592855));
#2125=CARTESIAN_POINT('',(20.773502833282,-5.00560343983409,40.8113234071455));
#2126=CARTESIAN_POINT('',(15.0000001413858,-15.0056034398341,40.8113234071455));
#2127=CARTESIAN_POINT('',(20.773502833282,-5.00560343983409,-119.188676592855));
#2128=CARTESIAN_POINT('',(20.773502833282,-5.00560343983409,-119.188676592855));
#2129=CARTESIAN_POINT('',(15.0000001413858,-15.0056034398341,-119.188676592855));
#2130=CARTESIAN_POINT('Origin',(15.0000001413858,-5.00560343983409,-119.188676592855));
#2131=CARTESIAN_POINT('',(-20.7735025505105,-5.00560343983409,40.8113234071455));
#2132=CARTESIAN_POINT('',(15.0000001413858,-5.00560343983409,40.8113234071455));
#2133=CARTESIAN_POINT('',(-20.7735025505105,-5.00560343983409,-119.188676592855));
#2134=CARTESIAN_POINT('',(-20.7735025505105,-5.00560343983409,-119.188676592855));
#2135=CARTESIAN_POINT('',(-14.9999998586142,-5.00560343983409,-119.188676592855));
#2136=CARTESIAN_POINT('Origin',(-14.9999998586142,-15.0056034398341,-119.188676592855));
#2137=CARTESIAN_POINT('',(-14.9999998586142,-15.0056034398341,40.8113234071455));
#2138=CARTESIAN_POINT('',(-14.9999998586142,-15.0056034398341,40.8113234071455));
#2139=CARTESIAN_POINT('',(-14.9999998586142,-15.0056034398341,-119.188676592855));
#2140=CARTESIAN_POINT('',(-14.9999998586142,-15.0056034398341,-119.188676592855));
#2141=CARTESIAN_POINT('',(-14.9999998586142,-15.0056034398341,-119.188676592855));
#2142=CARTESIAN_POINT('Origin',(-49.9999998586142,-15.0056034398341,-119.188676592855));
#2143=CARTESIAN_POINT('',(-49.9999998586142,-15.0056034398341,40.8113234071455));
#2144=CARTESIAN_POINT('',(-49.9999998586142,-15.0056034398341,-119.188676592855));
#2145=CARTESIAN_POINT('Origin',(1.41385779953466E-7,-15.0056034398341,-119.188676592855));
#2146=CARTESIAN_POINT('',(-48.9999998586142,28.9943965601659,-119.188676592855));
#2147=CARTESIAN_POINT('',(49.0000001413876,28.9943965606416,-119.188676592855));
#2148=CARTESIAN_POINT('Origin',(1.41385779953466E-7,-15.0056034398341,40.8113234071455));
#2149=CARTESIAN_POINT('Origin',(49.0000001413876,52.9943965606364,-89.1886765928545));
#2150=CARTESIAN_POINT('',(49.0000001413876,52.9943965606364,-89.1886765928545));
#2151=CARTESIAN_POINT('Origin',(49.0000001413876,-15.0056034398341,40.8113234071455));
#2152=CARTESIAN_POINT('Origin',(-48.9999998586142,52.994396560166,-89.1886765928545));
#2153=CARTESIAN_POINT('',(-48.9999998586142,52.994396560166,-89.1886765928545));
#2154=CARTESIAN_POINT('Origin',(-48.9999998586142,-15.0056034398341,40.8113234071455));
#2155=CARTESIAN_POINT('',(0.,0.,0.));
#2156=CARTESIAN_POINT('Origin',(-0.619834889991667,57.4408918778678,-9.99053328739284));
#2157=CARTESIAN_POINT('',(-0.619834889991667,41.4359646982476,-1.49053328739287));
#2158=CARTESIAN_POINT('',(-0.619834889991667,41.4359646982476,-18.4905332873928));
#2159=CARTESIAN_POINT('Ctrl Pts',(-0.619834889991664,41.4359646982476,-1.49053328739287));
#2160=CARTESIAN_POINT('Ctrl Pts',(-1.69251426133731,41.4186890416464,-1.49053328739286));
#2161=CARTESIAN_POINT('Ctrl Pts',(-2.83333550672754,41.3503146663282,-1.70589301181152));
#2162=CARTESIAN_POINT('Ctrl Pts',(-4.92696200368771,41.1358561238382,-2.57544700481013));
#2163=CARTESIAN_POINT('Ctrl Pts',(-5.880109476723,40.9922072228327,-3.22941616388057));
#2164=CARTESIAN_POINT('Ctrl Pts',(-7.38400452652566,40.7259525153024,-4.73446508972372));
#2165=CARTESIAN_POINT('Ctrl Pts',(-8.03690297146328,40.5856574031577,-5.68707722694506));
#2166=CARTESIAN_POINT('Ctrl Pts',(-8.90492499084854,40.387359614178,-7.77921932756061));
#2167=CARTESIAN_POINT('Ctrl Pts',(-9.11983488999165,40.332259216097,-8.91911200064825));
#2168=CARTESIAN_POINT('Ctrl Pts',(-9.11983488999165,40.332259216097,-9.99053328739285));
#2169=CARTESIAN_POINT('Ctrl Pts',(-9.11983488999165,40.332259216097,-11.0619545741374));
#2170=CARTESIAN_POINT('Ctrl Pts',(-8.90492499084854,40.387359614178,-12.2018472472251));
#2171=CARTESIAN_POINT('Ctrl Pts',(-8.03690297146328,40.5856574031577,-14.2939893478406));
#2172=CARTESIAN_POINT('Ctrl Pts',(-7.38400452652566,40.7259525153024,-15.246601485062));
#2173=CARTESIAN_POINT('Ctrl Pts',(-5.880109476723,40.9922072228327,-16.7516504109051));
#2174=CARTESIAN_POINT('Ctrl Pts',(-4.92696200368771,41.1358561238382,-17.4056195699756));
#2175=CARTESIAN_POINT('Ctrl Pts',(-2.83333550672754,41.3503146663282,-18.2751735629742));
#2176=CARTESIAN_POINT('Ctrl Pts',(-1.69251426133732,41.4186890416464,-18.4905332873928));
#2177=CARTESIAN_POINT('Ctrl Pts',(-0.619834889991667,41.4359646982476,-18.4905332873928));
#2178=CARTESIAN_POINT('',(-0.619834889991668,57.4408918778678,-18.4905332873928));
#2179=CARTESIAN_POINT('',(-0.619834889991668,57.4408918778678,-18.4905332873928));
#2180=CARTESIAN_POINT('Origin',(-0.619834889991667,57.4408918778678,-9.99053328739284));
#2181=CARTESIAN_POINT('Ctrl Pts',(-0.619834889991667,41.4359646982476,-18.4905332873928));
#2182=CARTESIAN_POINT('Ctrl Pts',(0.449797224212465,41.4531912783312,-18.4905332873928));
#2183=CARTESIAN_POINT('Ctrl Pts',(1.5892054277245,41.4218020260498,-18.2762675827069));
#2184=CARTESIAN_POINT('Ctrl Pts',(3.68206578130104,41.2758539577384,-17.4085452787979));
#2185=CARTESIAN_POINT('Ctrl Pts',(4.63575860476113,41.1637585877487,-16.755256589616));
#2186=CARTESIAN_POINT('Ctrl Pts',(6.14230817135067,40.9476179603983,-15.2497032680988));
#2187=CARTESIAN_POINT('Ctrl Pts',(6.79640351541145,40.8293540083924,-14.2956842723128));
#2188=CARTESIAN_POINT('Ctrl Pts',(7.66541391347513,40.6607235779339,-12.2017692944875));
#2189=CARTESIAN_POINT('Ctrl Pts',(7.88016511000832,40.6131682833795,-11.0615798711795));
#2190=CARTESIAN_POINT('Ctrl Pts',(7.88016511000832,40.6131682833795,-8.91948670360617));
#2191=CARTESIAN_POINT('Ctrl Pts',(7.66541391347513,40.6607235779339,-7.77929728029815));
#2192=CARTESIAN_POINT('Ctrl Pts',(6.79640351541145,40.8293540083924,-5.68538230247293));
#2193=CARTESIAN_POINT('Ctrl Pts',(6.14230817135067,40.9476179603983,-4.73136330668694));
#2194=CARTESIAN_POINT('Ctrl Pts',(4.63575860476114,41.1637585877487,-3.22580998516966));
#2195=CARTESIAN_POINT('Ctrl Pts',(3.68206578130104,41.2758539577384,-2.57252129598781));
#2196=CARTESIAN_POINT('Ctrl Pts',(1.5892054277245,41.4218020260498,-1.70479899207882));
#2197=CARTESIAN_POINT('Ctrl Pts',(0.449797224212467,41.4531912783312,-1.49053328739287));
#2198=CARTESIAN_POINT('Ctrl Pts',(-0.619834889991665,41.4359646982476,-1.49053328739287));
#2199=CARTESIAN_POINT('Origin',(27.9920812595258,-52.5591081221322,-29.9998965134939));
#2200=CARTESIAN_POINT('',(37.9920812595258,-52.5591081221322,10.0001034865061));
#2201=CARTESIAN_POINT('',(27.9920812595258,-52.5591081221322,10.0001034865061));
#2202=CARTESIAN_POINT('',(27.9920812595258,-52.5591081221322,10.0001034865061));
#2203=CARTESIAN_POINT('',(37.9920812595258,-52.5591081221322,-29.9998965134939));
#2204=CARTESIAN_POINT('',(37.9920812595258,-52.5591081221322,-29.9998965134939));
#2205=CARTESIAN_POINT('',(27.9920812595258,-52.5591081221322,-29.9998965134939));
#2206=CARTESIAN_POINT('',(27.9920812595258,-52.5591081221322,-29.9998965134939));
#2207=CARTESIAN_POINT('',(27.9920812595258,-52.5591081221322,-29.9998965134939));
#2208=CARTESIAN_POINT('Origin',(37.9920812595258,3.44089187786782,-29.9998965134939));
#2209=CARTESIAN_POINT('',(37.9920812595258,3.44089187786782,10.0001034865061));
#2210=CARTESIAN_POINT('',(37.9920812595258,3.44089187786782,10.0001034865061));
#2211=CARTESIAN_POINT('',(37.9920812595258,3.44089187786782,-29.9998965134939));
#2212=CARTESIAN_POINT('',(37.9920812595258,3.44089187786782,-29.9998965134939));
#2213=CARTESIAN_POINT('',(37.9920812595258,3.44089187786782,-29.9998965134939));
#2214=CARTESIAN_POINT('Origin',(-0.00791874047421016,3.44089187786782,-29.9998965134939));
#2215=CARTESIAN_POINT('',(-38.0079187404742,3.44089187786782,10.0001034865061));
#2216=CARTESIAN_POINT('Origin',(-0.00791874047421016,3.44089187786782,10.0001034865061));
#2217=CARTESIAN_POINT('',(-38.0079187404742,3.44089187786782,-29.9998965134939));
#2218=CARTESIAN_POINT('',(-38.0079187404742,3.44089187786782,-29.9998965134939));
#2219=CARTESIAN_POINT('Origin',(-0.00791874047421016,3.44089187786782,-29.9998965134939));
#2220=CARTESIAN_POINT('Origin',(-38.0079187404742,3.44089187786782,-29.9998965134939));
#2221=CARTESIAN_POINT('',(-38.0079187404742,-52.5591081221322,10.0001034865061));
#2222=CARTESIAN_POINT('',(-38.0079187404742,3.44089187786782,10.0001034865061));
#2223=CARTESIAN_POINT('',(-38.0079187404742,-52.5591081221322,-29.9998965134939));
#2224=CARTESIAN_POINT('',(-38.0079187404742,-52.5591081221322,-29.9998965134939));
#2225=CARTESIAN_POINT('',(-38.0079187404742,3.44089187786782,-29.9998965134939));
#2226=CARTESIAN_POINT('Origin',(-28.0079187404742,-52.5591081221322,-29.9998965134939));
#2227=CARTESIAN_POINT('',(-28.0079187404742,-52.5591081221322,10.0001034865061));
#2228=CARTESIAN_POINT('',(-28.0079187404742,-52.5591081221322,10.0001034865061));
#2229=CARTESIAN_POINT('',(-28.0079187404742,-52.5591081221322,-29.9998965134939));
#2230=CARTESIAN_POINT('',(-28.0079187404742,-52.5591081221322,-29.9998965134939));
#2231=CARTESIAN_POINT('',(-28.0079187404742,-52.5591081221322,-29.9998965134939));
#2232=CARTESIAN_POINT('Origin',(-28.0079187404742,-66.5591081221322,-29.9998965134939));
#2233=CARTESIAN_POINT('',(-28.0079187404742,-66.5591081221322,10.0001034865061));
#2234=CARTESIAN_POINT('',(-28.0079187404742,-66.5591081221322,10.0001034865061));
#2235=CARTESIAN_POINT('',(-28.0079187404742,-66.5591081221322,-29.9998965134939));
#2236=CARTESIAN_POINT('',(-28.0079187404742,-66.5591081221322,-29.9998965134939));
#2237=CARTESIAN_POINT('',(-28.0079187404742,-66.5591081221322,-29.9998965134939));
#2238=CARTESIAN_POINT('Origin',(-50.0079187404742,-66.5591081221322,-29.9998965134939));
#2239=CARTESIAN_POINT('',(-44.0079187404742,-66.5591081221322,10.0001034865061));
#2240=CARTESIAN_POINT('',(-50.0079187404742,-66.5591081221322,10.0001034865061));
#2241=CARTESIAN_POINT('',(-44.0079187404742,-66.5591081221322,-29.9998965134939));
#2242=CARTESIAN_POINT('',(-44.0079187404742,-66.5591081221322,-29.9998965134939));
#2243=CARTESIAN_POINT('',(-50.0079187404742,-66.5591081221322,-29.9998965134939));
#2244=CARTESIAN_POINT('Origin',(-50.0079187404742,3.44089187786782,-29.9998965134939));
#2245=CARTESIAN_POINT('',(-50.0079187404742,3.44089187786783,-29.9998965134939));
#2246=CARTESIAN_POINT('',(-50.0079187404742,-60.5591081221322,-29.9998965134939));
#2247=CARTESIAN_POINT('',(-50.0079187404742,3.44089187786782,-29.9998965134939));
#2248=CARTESIAN_POINT('',(-50.0079187404742,-60.5591081221322,10.0001034865061));
#2249=CARTESIAN_POINT('',(-50.0079187404742,-60.5591081221322,-29.9998965134939));
#2250=CARTESIAN_POINT('',(-50.0079187404742,3.44089187786783,10.0001034865061));
#2251=CARTESIAN_POINT('',(-50.0079187404742,3.44089187786782,10.0001034865061));
#2252=CARTESIAN_POINT('',(-50.0079187404742,3.44089187786783,-29.9998965134939));
#2253=CARTESIAN_POINT('Origin',(-0.00791874047421016,3.44089187786782,-29.9998965134939));
#2254=CARTESIAN_POINT('',(-18.7579187404742,49.7921324222157,10.0001034865061));
#2255=CARTESIAN_POINT('Origin',(-0.00791874047421016,3.44089187786782,10.0001034865061));
#2256=CARTESIAN_POINT('',(-18.7579187404742,49.7921324222157,-29.9998965134939));
#2257=CARTESIAN_POINT('',(-18.7579187404742,49.7921324222157,-29.9998965134939));
#2258=CARTESIAN_POINT('Origin',(-0.00791874047421016,3.44089187786782,-29.9998965134939));
#2259=CARTESIAN_POINT('Origin',(-15.0079187404742,57.4408918778678,-29.9998965134939));
#2260=CARTESIAN_POINT('',(-15.0079187404742,57.4408918778678,-29.9998965134939));
#2261=CARTESIAN_POINT('',(-15.0079187404742,55.3542812875375,-29.9998965134939));
#2262=CARTESIAN_POINT('',(-15.0079187404742,57.4408918778678,-29.9998965134939));
#2263=CARTESIAN_POINT('',(-15.0079187404742,55.3542812875375,10.0001034865061));
#2264=CARTESIAN_POINT('',(-15.0079187404742,55.3542812875375,10.0001034865061));
#2265=CARTESIAN_POINT('',(-15.0079187404742,57.4408918778678,10.0001034865061));
#2266=CARTESIAN_POINT('',(-15.0079187404742,57.4408918778678,10.0001034865061));
#2267=CARTESIAN_POINT('',(-15.0079187404742,57.4408918778678,-29.9998965134939));
#2268=CARTESIAN_POINT('Origin',(-0.00791874047421016,57.4408918778678,-29.9998965134939));
#2269=CARTESIAN_POINT('',(14.9920812595258,57.4408918778678,10.0001034865061));
#2270=CARTESIAN_POINT('',(-0.00791874047421016,57.4408918778678,10.0001034865061));
#2271=CARTESIAN_POINT('',(14.9920812595258,57.4408918778678,-29.9998965134939));
#2272=CARTESIAN_POINT('',(14.9920812595258,57.4408918778678,-29.9998965134939));
#2273=CARTESIAN_POINT('',(-0.00791874047421016,57.4408918778678,-29.9998965134939));
#2274=CARTESIAN_POINT('Origin',(14.9920812595258,57.4408918778678,-29.9998965134939));
#2275=CARTESIAN_POINT('',(14.9920812595258,55.3542812875375,10.0001034865061));
#2276=CARTESIAN_POINT('',(14.9920812595258,57.4408918778678,10.0001034865061));
#2277=CARTESIAN_POINT('',(14.9920812595258,55.3542812875375,-29.9998965134939));
#2278=CARTESIAN_POINT('',(14.9920812595258,55.3542812875375,-29.9998965134939));
#2279=CARTESIAN_POINT('',(14.9920812595258,57.4408918778678,-29.9998965134939));
#2280=CARTESIAN_POINT('Origin',(-0.00791874047421016,3.44089187786782,-29.9998965134939));
#2281=CARTESIAN_POINT('',(49.9920812595258,3.44089187786782,-29.9998965134939));
#2282=CARTESIAN_POINT('',(18.7420812595258,49.7921324222157,-29.9998965134939));
#2283=CARTESIAN_POINT('Origin',(-0.00791874047421016,3.44089187786782,-29.9998965134939));
#2284=CARTESIAN_POINT('',(18.7420812595258,49.7921324222157,10.0001034865061));
#2285=CARTESIAN_POINT('',(18.7420812595258,49.7921324222157,-29.9998965134939));
#2286=CARTESIAN_POINT('',(49.9920812595258,3.44089187786782,10.0001034865061));
#2287=CARTESIAN_POINT('Origin',(-0.00791874047421016,3.44089187786782,10.0001034865061));
#2288=CARTESIAN_POINT('',(49.9920812595258,3.44089187786782,-29.9998965134939));
#2289=CARTESIAN_POINT('Origin',(49.9920812595258,-66.5591081221322,-29.9998965134939));
#2290=CARTESIAN_POINT('',(49.9920812595258,-60.5591081221322,10.0001034865061));
#2291=CARTESIAN_POINT('',(49.9920812595258,-66.5591081221322,10.0001034865061));
#2292=CARTESIAN_POINT('',(49.9920812595258,-60.5591081221322,-29.9998965134939));
#2293=CARTESIAN_POINT('',(49.9920812595258,-60.5591081221322,-29.9998965134939));
#2294=CARTESIAN_POINT('',(49.9920812595258,-66.5591081221322,-29.9998965134939));
#2295=CARTESIAN_POINT('Origin',(49.9920812595258,-66.5591081221322,-29.9998965134939));
#2296=CARTESIAN_POINT('',(27.9920812595258,-66.5591081221322,-29.9998965134939));
#2297=CARTESIAN_POINT('',(43.9920812595258,-66.5591081221322,-29.9998965134939));
#2298=CARTESIAN_POINT('',(49.9920812595258,-66.5591081221322,-29.9998965134939));
#2299=CARTESIAN_POINT('',(43.9920812595258,-66.5591081221322,10.0001034865061));
#2300=CARTESIAN_POINT('',(43.9920812595258,-66.5591081221322,-29.9998965134939));
#2301=CARTESIAN_POINT('',(27.9920812595258,-66.5591081221322,10.0001034865061));
#2302=CARTESIAN_POINT('',(49.9920812595258,-66.5591081221322,10.0001034865061));
#2303=CARTESIAN_POINT('',(27.9920812595258,-66.5591081221322,-29.9998965134939));
#2304=CARTESIAN_POINT('Origin',(27.9920812595258,-66.5591081221322,-29.9998965134939));
#2305=CARTESIAN_POINT('',(27.9920812595258,-66.5591081221322,10.0001034865061));
#2306=CARTESIAN_POINT('',(27.9920812595258,-66.5591081221322,-29.9998965134939));
#2307=CARTESIAN_POINT('Origin',(-0.00791874047421016,3.44089187786782,-29.9998965134939));
#2308=CARTESIAN_POINT('Origin',(43.9920812595258,-60.5591081221322,-29.9998965134939));
#2309=CARTESIAN_POINT('Origin',(-44.0079187404742,-60.5591081221322,-29.9998965134939));
#2310=CARTESIAN_POINT('Origin',(-21.0079187404742,55.3542812875375,-29.9998965134939));
#2311=CARTESIAN_POINT('Origin',(20.9920812595258,55.3542812875375,-29.9998965134939));
#2312=CARTESIAN_POINT('Origin',(-0.00791874047421016,3.44089187786782,10.0001034865061));
#2313=CARTESIAN_POINT('Origin',(43.9920812595258,-60.5591081221322,10.0001034865061));
#2314=CARTESIAN_POINT('Origin',(20.9920812595258,55.3542812875375,10.0001034865061));
#2315=CARTESIAN_POINT('Origin',(-21.0079187404742,55.3542812875375,10.0001034865061));
#2316=CARTESIAN_POINT('Origin',(-44.0079187404742,-60.5591081221322,10.0001034865061));
#2317=CARTESIAN_POINT('Origin',(43.9920812595258,-60.5591081221322,-29.9998965134939));
#2318=CARTESIAN_POINT('Origin',(-44.0079187404742,-60.5591081221322,-29.9998965134939));
#2319=CARTESIAN_POINT('Origin',(-21.0079187404742,55.3542812875375,-29.9998965134939));
#2320=CARTESIAN_POINT('Origin',(20.9920812595258,55.3542812875375,-29.9998965134939));
#2321=CARTESIAN_POINT('',(0.,0.,0.));
#2322=CARTESIAN_POINT('Origin',(-3.0679035930424E-16,0.,-105.));
#2323=CARTESIAN_POINT('',(-30.,-3.67394039744206E-15,35.));
#2324=CARTESIAN_POINT('Origin',(-3.0679035930424E-16,0.,35.));
#2325=CARTESIAN_POINT('',(-30.,-3.67394039744206E-15,-105.));
#2326=CARTESIAN_POINT('',(-30.,-3.67394039744206E-15,-105.));
#2327=CARTESIAN_POINT('Origin',(-3.0679035930424E-16,0.,-105.));
#2328=CARTESIAN_POINT('Origin',(-3.0679035930424E-16,0.,-105.));
#2329=CARTESIAN_POINT('Origin',(-3.0679035930424E-16,0.,35.));
#2330=CARTESIAN_POINT('',(0.,0.,0.));
#2331=CARTESIAN_POINT('Origin',(24.205110751768,1.03590535159927E-6,1.40295421642658E-16));
#2332=CARTESIAN_POINT('',(24.205110751768,1.03590535264022E-6,-8.5));
#2333=CARTESIAN_POINT('',(24.205110751768,1.03590535055832E-6,8.5));
#2334=CARTESIAN_POINT('Origin',(24.205110751768,1.03590535159927E-6,1.40295421642658E-16));
#2335=CARTESIAN_POINT('Origin',(24.205110751768,1.03590535159927E-6,1.40295421642658E-16));
#2336=CARTESIAN_POINT('',(23.6384440851014,1.03590535048892E-6,9.06666666666667));
#2337=CARTESIAN_POINT('Origin',(24.205110751768,1.03590535048892E-6,9.06666666666667));
#2338=CARTESIAN_POINT('Origin',(23.6384440851014,1.03590535159927E-6,1.40295421642658E-16));
#2339=CARTESIAN_POINT('Origin',(13.0134440851014,1.03590535159927E-6,1.40295421642658E-16));
#2340=CARTESIAN_POINT('',(23.0717774184347,-11.0418228623462,6.37500000000003));
#2341=CARTESIAN_POINT('',(23.0717774184347,1.03590535159927E-6,12.75));
#2342=CARTESIAN_POINT('Origin',(23.0717774184347,1.03590535159927E-6,1.40295421642658E-16));
#2343=CARTESIAN_POINT('',(23.0717774184347,-11.0418228623462,-6.375));
#2344=CARTESIAN_POINT('Origin',(23.0717774184347,1.03590535159927E-6,1.40295421642658E-16));
#2345=CARTESIAN_POINT('',(23.0717774184347,1.03590535159927E-6,-12.75));
#2346=CARTESIAN_POINT('Origin',(23.0717774184347,1.03590535159927E-6,1.40295421642658E-16));
#2347=CARTESIAN_POINT('',(23.6384440851014,1.03590535003785E-6,-12.75));
#2348=CARTESIAN_POINT('',(13.0134440851014,1.03590535003785E-6,-12.75));
#2349=CARTESIAN_POINT('Origin',(23.6384440851014,1.03590535159927E-6,1.40295421642658E-16));
#2350=CARTESIAN_POINT('',(23.0717774184347,11.0418249341569,-6.37500000000002));
#2351=CARTESIAN_POINT('Origin',(23.0717774184347,1.03590535159927E-6,1.40295421642658E-16));
#2352=CARTESIAN_POINT('',(23.0717774184347,11.0418249341569,6.37500000000001));
#2353=CARTESIAN_POINT('Origin',(23.0717774184347,1.03590535159927E-6,1.40295421642658E-16));
#2354=CARTESIAN_POINT('Origin',(23.0717774184347,1.03590535159927E-6,1.40295421642658E-16));
#2355=CARTESIAN_POINT('Origin',(87.3884440851014,1.03590535159927E-6,1.40295421642658E-16));
#2356=CARTESIAN_POINT('',(86.221110751768,1.03590535055832E-6,-8.50000000000001));
#2357=CARTESIAN_POINT('Origin',(86.221110751768,1.03590535159927E-6,1.40295421642658E-16));
#2358=CARTESIAN_POINT('',(87.3884440851014,1.03590535070128E-6,-7.33266666666667));
#2359=CARTESIAN_POINT('',(87.3884440851014,1.03590535070128E-6,-7.33266666666667));
#2360=CARTESIAN_POINT('Origin',(87.3884440851014,1.03590535159927E-6,1.40295421642658E-16));
#2361=CARTESIAN_POINT('Origin',(13.0134440851014,1.03590535159927E-6,1.40295421642658E-16));
#2362=CARTESIAN_POINT('',(13.0134440851014,1.03590535055832E-6,-8.5));
#2363=CARTESIAN_POINT('Origin',(23.6384440851014,14.7224329002408,-6.38708764143874E-16));
#2364=CARTESIAN_POINT('Origin',(87.3884440851014,1.03590535159927E-6,1.40295421642658E-16));
#2365=CARTESIAN_POINT('Origin',(23.0717774184347,12.7500010359054,1.40295421642658E-16));
#2366=CARTESIAN_POINT('',(23.0717774184347,7.36121696807307,-12.75));
#2367=CARTESIAN_POINT('',(23.0717774184347,7.36121696807307,-12.75));
#2368=CARTESIAN_POINT('',(23.0717774184347,7.36121696807307,-12.75));
#2369=CARTESIAN_POINT('Origin',(23.0717774184347,12.7500010359054,1.40295421642658E-16));
#2370=CARTESIAN_POINT('',(23.0717774184347,14.7224329002408,1.40295421642658E-16));
#2371=CARTESIAN_POINT('',(23.0717774184347,7.36121696807307,-12.75));
#2372=CARTESIAN_POINT('',(23.0717774184347,14.7224329002408,1.40295421642658E-16));
#2373=CARTESIAN_POINT('Origin',(23.0717774184347,12.7500010359054,1.40295421642658E-16));
#2374=CARTESIAN_POINT('',(23.0717774184347,7.36121696807307,12.75));
#2375=CARTESIAN_POINT('',(23.0717774184347,14.7224329002408,1.40295421642658E-16));
#2376=CARTESIAN_POINT('',(23.0717774184347,7.36121696807307,12.75));
#2377=CARTESIAN_POINT('Origin',(23.0717774184347,12.7500010359054,1.40295421642658E-16));
#2378=CARTESIAN_POINT('',(23.0717774184347,-7.36121489626235,12.75));
#2379=CARTESIAN_POINT('',(23.0717774184347,7.36121696807307,12.75));
#2380=CARTESIAN_POINT('',(23.0717774184347,-14.7224308284301,1.40295421642658E-16));
#2381=CARTESIAN_POINT('Origin',(23.0717774184347,12.7500010359054,1.40295421642658E-16));
#2382=CARTESIAN_POINT('',(23.0717774184347,-14.7224308284301,2.59782034594314E-15));
#2383=CARTESIAN_POINT('',(23.0717774184347,-14.7224308284301,1.40295421642658E-16));
#2384=CARTESIAN_POINT('',(23.0717774184347,-7.36121489626239,-12.75));
#2385=CARTESIAN_POINT('Origin',(23.0717774184347,12.7500010359054,1.40295421642658E-16));
#2386=CARTESIAN_POINT('',(23.0717774184347,-7.36121489626239,-12.75));
#2387=CARTESIAN_POINT('',(23.0717774184347,-7.36121489626239,-12.75));
#2388=CARTESIAN_POINT('',(23.0717774184347,7.36121696807307,-12.75));
#2389=CARTESIAN_POINT('Origin',(13.0134440851014,14.7224329002408,-6.38708764143874E-16));
#2390=CARTESIAN_POINT('',(13.0134440851014,1.03590535159927E-6,-12.75));
#2391=CARTESIAN_POINT('',(13.0134440851014,11.0418249341569,-6.37500000000001));
#2392=CARTESIAN_POINT('Origin',(13.0134440851014,1.03590535159927E-6,1.40295421642658E-16));
#2393=CARTESIAN_POINT('',(13.0134440851014,-11.0418228623462,-6.375));
#2394=CARTESIAN_POINT('Origin',(13.0134440851014,1.03590535159927E-6,1.40295421642658E-16));
#2395=CARTESIAN_POINT('',(13.0134440851014,-11.0418228623462,6.37500000000003));
#2396=CARTESIAN_POINT('Origin',(13.0134440851014,1.03590535159927E-6,1.40295421642658E-16));
#2397=CARTESIAN_POINT('',(13.0134440851014,1.03590534947099E-6,12.75));
#2398=CARTESIAN_POINT('Origin',(13.0134440851014,1.03590535159927E-6,1.40295421642658E-16));
#2399=CARTESIAN_POINT('',(13.0134440851014,11.0418249341569,6.37500000000001));
#2400=CARTESIAN_POINT('Origin',(13.0134440851014,1.03590535159927E-6,1.40295421642658E-16));
#2401=CARTESIAN_POINT('Origin',(13.0134440851014,1.03590535159927E-6,1.40295421642658E-16));
#2402=CARTESIAN_POINT('Origin',(13.0134440851014,1.03590535159927E-6,1.40295421642658E-16));
#2403=CARTESIAN_POINT('',(14.1522281529336,14.7224329002408,-1.64721472015358E-16));
#2404=CARTESIAN_POINT('Ctrl Pts',(13.0134440851014,11.0418249341569,6.37500000000002));
#2405=CARTESIAN_POINT('Ctrl Pts',(13.0134440851014,12.7500010359066,3.4163522034947));
#2406=CARTESIAN_POINT('Ctrl Pts',(14.1522281529354,14.7224329002439,-5.29990213494028E-12));
#2407=CARTESIAN_POINT('Ctrl Pts',(14.1522281529354,14.7224329002439,5.31028445688728E-12));
#2408=CARTESIAN_POINT('Ctrl Pts',(13.0134440851014,12.7500010359066,-3.41635220349469));
#2409=CARTESIAN_POINT('Ctrl Pts',(13.0134440851014,11.0418249341569,-6.37500000000001));
#2410=CARTESIAN_POINT('Origin',(13.0134440851014,1.03590535159927E-6,1.40295421642658E-16));
#2411=CARTESIAN_POINT('',(14.1522281529336,7.36121696807307,12.75));
#2412=CARTESIAN_POINT('Ctrl Pts',(13.0134440851014,1.03590535214333E-6,
12.75));
#2413=CARTESIAN_POINT('Ctrl Pts',(13.0134440851014,3.41635323940462,12.75));
#2414=CARTESIAN_POINT('Ctrl Pts',(14.1522281529354,7.3612169680792,12.75));
#2415=CARTESIAN_POINT('Ctrl Pts',(14.1522281529354,7.36121696807001,12.7500000000053));
#2416=CARTESIAN_POINT('Ctrl Pts',(13.0134440851014,9.3336488324073,9.33364779650533));
#2417=CARTESIAN_POINT('Ctrl Pts',(13.0134440851014,11.0418249341569,6.37500000000002));
#2418=CARTESIAN_POINT('Origin',(13.0134440851014,1.03590535159927E-6,1.40295421642658E-16));
#2419=CARTESIAN_POINT('',(14.1522281529336,-7.36121489626235,12.75));
#2420=CARTESIAN_POINT('Ctrl Pts',(14.1522281529354,-7.36121489626846,12.75));
#2421=CARTESIAN_POINT('Ctrl Pts',(13.0134440851014,-3.41635116759391,12.75));
#2422=CARTESIAN_POINT('Ctrl Pts',(13.0134440851014,1.03590535214333E-6,
12.75));
#2423=CARTESIAN_POINT('Ctrl Pts',(13.0134440851014,-11.0418228623462,6.37500000000002));
#2424=CARTESIAN_POINT('Ctrl Pts',(13.0134440851014,-9.33364676059658,9.33364779650533));
#2425=CARTESIAN_POINT('Ctrl Pts',(14.1522281529354,-7.36121489625929,12.7500000000053));
#2426=CARTESIAN_POINT('Origin',(13.0134440851014,1.03590535159927E-6,1.40295421642658E-16));
#2427=CARTESIAN_POINT('',(14.1522281529336,-14.7224308284301,-2.39052969952593E-16));
#2428=CARTESIAN_POINT('Ctrl Pts',(14.1522281529354,-14.7224308284332,-5.3009950109347E-12));
#2429=CARTESIAN_POINT('Ctrl Pts',(13.0134440851014,-12.7499989640959,3.4163522034947));
#2430=CARTESIAN_POINT('Ctrl Pts',(13.0134440851014,-11.0418228623462,6.37500000000002));
#2431=CARTESIAN_POINT('Ctrl Pts',(13.0134440851014,-11.0418228623462,-6.375));
#2432=CARTESIAN_POINT('Ctrl Pts',(13.0134440851014,-12.7499989640959,-3.41635220349468));
#2433=CARTESIAN_POINT('Ctrl Pts',(14.1522281529354,-14.7224308284332,5.2955306309626E-12));
#2434=CARTESIAN_POINT('Origin',(13.0134440851014,1.03590535159927E-6,1.40295421642658E-16));
#2435=CARTESIAN_POINT('',(14.1522281529336,7.36121696807307,-12.75));
#2436=CARTESIAN_POINT('Ctrl Pts',(13.0134440851014,11.0418249341569,-6.37500000000001));
#2437=CARTESIAN_POINT('Ctrl Pts',(13.0134440851014,9.3336488324073,-9.33364779650533));
#2438=CARTESIAN_POINT('Ctrl Pts',(14.1522281529354,7.36121696807001,-12.7500000000053));
#2439=CARTESIAN_POINT('Ctrl Pts',(14.1522281529354,7.36121696807918,-12.75));
#2440=CARTESIAN_POINT('Ctrl Pts',(13.0134440851014,3.41635323940461,-12.75));
#2441=CARTESIAN_POINT('Ctrl Pts',(13.0134440851014,1.03590534199922E-6,
-12.75));
#2442=CARTESIAN_POINT('Origin',(13.0134440851014,1.03590535159927E-6,1.40295421642658E-16));
#2443=CARTESIAN_POINT('',(14.1522281529336,-7.36121489626239,-12.75));
#2444=CARTESIAN_POINT('Ctrl Pts',(14.1522281529354,-7.36121489625932,-12.7500000000053));
#2445=CARTESIAN_POINT('Ctrl Pts',(13.0134440851014,-9.33364676059661,-9.33364779650532));
#2446=CARTESIAN_POINT('Ctrl Pts',(13.0134440851014,-11.0418228623462,-6.375));
#2447=CARTESIAN_POINT('Ctrl Pts',(13.0134440851014,1.03590534199922E-6,
-12.75));
#2448=CARTESIAN_POINT('Ctrl Pts',(13.0134440851014,-3.41635116759393,-12.75));
#2449=CARTESIAN_POINT('Ctrl Pts',(14.1522281529354,-7.3612148962685,-12.75));
#2450=CARTESIAN_POINT('Origin',(23.6384440851014,7.36121696807307,-12.75));
#2451=CARTESIAN_POINT('',(23.6384440851014,-7.36121489626239,-12.75));
#2452=CARTESIAN_POINT('',(23.6384440851014,7.36121696807307,-12.75));
#2453=CARTESIAN_POINT('Origin',(23.6384440851014,-7.36121489626239,-12.75));
#2454=CARTESIAN_POINT('',(23.6384440851014,-14.7224308284301,1.40295421642658E-16));
#2455=CARTESIAN_POINT('Origin',(23.6384440851014,-14.7224308284301,1.40295421642658E-16));
#2456=CARTESIAN_POINT('',(23.6384440851014,-7.36121489626235,12.75));
#2457=CARTESIAN_POINT('Origin',(23.6384440851014,7.36121696807307,12.75));
#2458=CARTESIAN_POINT('',(23.6384440851014,7.36121696807307,12.75));
#2459=CARTESIAN_POINT('Origin',(23.6384440851014,14.7224329002408,1.40295421642658E-16));
#2460=CARTESIAN_POINT('',(23.6384440851014,14.7224329002408,1.40295421642658E-16));
#2461=CARTESIAN_POINT('Origin',(23.6384440851014,7.36121696807307,-12.75));
#2462=CARTESIAN_POINT('',(-2.634940816759,-21.0887012675017,120.));
#2463=CARTESIAN_POINT('',(-3.12702193489719,60.4648034147964,70.8112199206394));
#2464=CARTESIAN_POINT('',(-2.63494067560857,49.3321021640924,105.811323407145));
#2465=CARTESIAN_POINT('',(-3.74685581100718,166.704139377766,60.8206868457173));
#2466=UNCERTAINTY_MEASURE_WITH_UNIT(LENGTH_MEASURE(0.01),#2478,
'DISTANCE_ACCURACY_VALUE',
'Maximum model space distance between geometric entities at asserted c
onnectivities');
#2467=UNCERTAINTY_MEASURE_WITH_UNIT(LENGTH_MEASURE(0.01),#2478,
'DISTANCE_ACCURACY_VALUE',
'Maximum model space distance between geometric entities at asserted c
onnectivities');
#2468=UNCERTAINTY_MEASURE_WITH_UNIT(LENGTH_MEASURE(0.01),#2478,
'DISTANCE_ACCURACY_VALUE',
'Maximum model space distance between geometric entities at asserted c
onnectivities');
#2469=UNCERTAINTY_MEASURE_WITH_UNIT(LENGTH_MEASURE(0.01),#2478,
'DISTANCE_ACCURACY_VALUE',
'Maximum model space distance between geometric entities at asserted c
onnectivities');
#2470=UNCERTAINTY_MEASURE_WITH_UNIT(LENGTH_MEASURE(0.01),#2478,
'DISTANCE_ACCURACY_VALUE',
'Maximum model space distance between geometric entities at asserted c
onnectivities');
#2471=UNCERTAINTY_MEASURE_WITH_UNIT(LENGTH_MEASURE(0.01),#2478,
'DISTANCE_ACCURACY_VALUE',
'Maximum model space distance between geometric entities at asserted c
onnectivities');
#2472=(
GEOMETRIC_REPRESENTATION_CONTEXT(3)
GLOBAL_UNCERTAINTY_ASSIGNED_CONTEXT((#2466))
GLOBAL_UNIT_ASSIGNED_CONTEXT((#2478,#2480,#2481))
REPRESENTATION_CONTEXT('','3D')
);
#2473=(
GEOMETRIC_REPRESENTATION_CONTEXT(3)
GLOBAL_UNCERTAINTY_ASSIGNED_CONTEXT((#2467))
GLOBAL_UNIT_ASSIGNED_CONTEXT((#2478,#2480,#2481))
REPRESENTATION_CONTEXT('','3D')
);
#2474=(
GEOMETRIC_REPRESENTATION_CONTEXT(3)
GLOBAL_UNCERTAINTY_ASSIGNED_CONTEXT((#2468))
GLOBAL_UNIT_ASSIGNED_CONTEXT((#2478,#2480,#2481))
REPRESENTATION_CONTEXT('','3D')
);
#2475=(
GEOMETRIC_REPRESENTATION_CONTEXT(3)
GLOBAL_UNCERTAINTY_ASSIGNED_CONTEXT((#2469))
GLOBAL_UNIT_ASSIGNED_CONTEXT((#2478,#2480,#2481))
REPRESENTATION_CONTEXT('','3D')
);
#2476=(
GEOMETRIC_REPRESENTATION_CONTEXT(3)
GLOBAL_UNCERTAINTY_ASSIGNED_CONTEXT((#2470))
GLOBAL_UNIT_ASSIGNED_CONTEXT((#2478,#2480,#2481))
REPRESENTATION_CONTEXT('','3D')
);
#2477=(
GEOMETRIC_REPRESENTATION_CONTEXT(3)
GLOBAL_UNCERTAINTY_ASSIGNED_CONTEXT((#2471))
GLOBAL_UNIT_ASSIGNED_CONTEXT((#2478,#2480,#2481))
REPRESENTATION_CONTEXT('','3D')
);
#2478=(
LENGTH_UNIT()
NAMED_UNIT(*)
SI_UNIT(.MILLI.,.METRE.)
);
#2479=(
LENGTH_UNIT()
NAMED_UNIT(*)
SI_UNIT($,.METRE.)
);
#2480=(
NAMED_UNIT(*)
PLANE_ANGLE_UNIT()
SI_UNIT($,.RADIAN.)
);
#2481=(
NAMED_UNIT(*)
SI_UNIT($,.STERADIAN.)
SOLID_ANGLE_UNIT()
);
#2482=SHAPE_DEFINITION_REPRESENTATION(#2487,#2496);
#2483=SHAPE_DEFINITION_REPRESENTATION(#2488,#2497);
#2484=SHAPE_DEFINITION_REPRESENTATION(#2489,#2498);
#2485=SHAPE_DEFINITION_REPRESENTATION(#2490,#2499);
#2486=SHAPE_DEFINITION_REPRESENTATION(#2491,#2500);
#2487=PRODUCT_DEFINITION_SHAPE('',$,#2502);
#2488=PRODUCT_DEFINITION_SHAPE('',$,#2503);
#2489=PRODUCT_DEFINITION_SHAPE('',$,#2504);
#2490=PRODUCT_DEFINITION_SHAPE('',$,#2505);
#2491=PRODUCT_DEFINITION_SHAPE('',$,#2506);
#2492=PRODUCT_DEFINITION_SHAPE($,$,#23);
#2493=PRODUCT_DEFINITION_SHAPE($,$,#24);
#2494=PRODUCT_DEFINITION_SHAPE($,$,#25);
#2495=PRODUCT_DEFINITION_SHAPE($,$,#26);
#2496=SHAPE_REPRESENTATION('',(#1476,#1596,#1597,#1598,#1599),#2472);
#2497=SHAPE_REPRESENTATION('',(#1477),#2473);
#2498=SHAPE_REPRESENTATION('',(#1506),#2474);
#2499=SHAPE_REPRESENTATION('',(#1545),#2475);
#2500=SHAPE_REPRESENTATION('',(#1551),#2476);
#2501=PRODUCT_DEFINITION_CONTEXT('part definition',#2518,'design');
#2502=PRODUCT_DEFINITION('MAT-002','MAT-002',#2507,#2501);
#2503=PRODUCT_DEFINITION('V-Block','V-Block',#2508,#2501);
#2504=PRODUCT_DEFINITION('Clamp','Clamp',#2509,#2501);
#2505=PRODUCT_DEFINITION('Round Bar','Round Bar',#2510,#2501);
#2506=PRODUCT_DEFINITION('Hex Screw Grade AB ISO',
'Hex Screw Grade AB ISO',#2511,#2501);
#2507=PRODUCT_DEFINITION_FORMATION('',$,#2520);
#2508=PRODUCT_DEFINITION_FORMATION('',$,#2521);
#2509=PRODUCT_DEFINITION_FORMATION('',$,#2522);
#2510=PRODUCT_DEFINITION_FORMATION('',$,#2523);
#2511=PRODUCT_DEFINITION_FORMATION('',$,#2524);
#2512=PRODUCT_RELATED_PRODUCT_CATEGORY('MAT-002','MAT-002',(#2520));
#2513=PRODUCT_RELATED_PRODUCT_CATEGORY('V-Block','V-Block',(#2521));
#2514=PRODUCT_RELATED_PRODUCT_CATEGORY('Clamp','Clamp',(#2522));
#2515=PRODUCT_RELATED_PRODUCT_CATEGORY('Round Bar','Round Bar',(#2523));
#2516=PRODUCT_RELATED_PRODUCT_CATEGORY('Hex Screw Grade AB ISO',
'Hex Screw Grade AB ISO',(#2524));
#2517=APPLICATION_PROTOCOL_DEFINITION('international standard',
'automotive_design',2009,#2518);
#2518=APPLICATION_CONTEXT(
'Core Data for Automotive Mechanical Design Process');
#2519=PRODUCT_CONTEXT('part definition',#2518,'mechanical');
#2520=PRODUCT('MAT-002','MAT-002','STEP AP214',(#2519));
#2521=PRODUCT('V-Block','V-Block',$,(#2519));
#2522=PRODUCT('Clamp','Clamp',$,(#2519));
#2523=PRODUCT('Round Bar','Round Bar',$,(#2519));
#2524=PRODUCT('Hex Screw Grade AB ISO','Hex Screw Grade AB ISO',$,(#2519));
#2525=PRESENTATION_STYLE_ASSIGNMENT((#2530));
#2526=PRESENTATION_STYLE_ASSIGNMENT((#2531));
#2527=PRESENTATION_STYLE_ASSIGNMENT((#2532));
#2528=PRESENTATION_STYLE_ASSIGNMENT((#2533));
#2529=PRESENTATION_STYLE_ASSIGNMENT((#2534));
#2530=SURFACE_STYLE_USAGE(.BOTH.,#2535);
#2531=SURFACE_STYLE_USAGE(.BOTH.,#2536);
#2532=SURFACE_STYLE_USAGE(.BOTH.,#2537);
#2533=SURFACE_STYLE_USAGE(.BOTH.,#2538);
#2534=SURFACE_STYLE_USAGE(.BOTH.,#2539);
#2535=SURFACE_SIDE_STYLE('',(#2540));
#2536=SURFACE_SIDE_STYLE('',(#2541));
#2537=SURFACE_SIDE_STYLE('',(#2542));
#2538=SURFACE_SIDE_STYLE('',(#2543));
#2539=SURFACE_SIDE_STYLE('',(#2544));
#2540=SURFACE_STYLE_FILL_AREA(#2545);
#2541=SURFACE_STYLE_FILL_AREA(#2546);
#2542=SURFACE_STYLE_FILL_AREA(#2547);
#2543=SURFACE_STYLE_FILL_AREA(#2548);
#2544=SURFACE_STYLE_FILL_AREA(#2549);
#2545=FILL_AREA_STYLE('Steel - Satin',(#2550));
#2546=FILL_AREA_STYLE('Opaque(97,158,199)',(#2551));
#2547=FILL_AREA_STYLE('Opaque(61,176,222)',(#2552));
#2548=FILL_AREA_STYLE('Opaque(227,224,212)',(#2553));
#2549=FILL_AREA_STYLE('Opaque(31,36,43)',(#2554));
#2550=FILL_AREA_STYLE_COLOUR('Steel - Satin',#2555);
#2551=FILL_AREA_STYLE_COLOUR('Opaque(97,158,199)',#2556);
#2552=FILL_AREA_STYLE_COLOUR('Opaque(61,176,222)',#2557);
#2553=FILL_AREA_STYLE_COLOUR('Opaque(227,224,212)',#2558);
#2554=FILL_AREA_STYLE_COLOUR('Opaque(31,36,43)',#2559);
#2555=COLOUR_RGB('Steel - Satin',0.627450980392157,0.627450980392157,0.627450980392157);
#2556=COLOUR_RGB('Opaque(97,158,199)',0.380392156862745,0.619607843137255,
0.780392156862745);
#2557=COLOUR_RGB('Opaque(61,176,222)',0.23921568627451,0.690196078431373,
0.870588235294118);
#2558=COLOUR_RGB('Opaque(227,224,212)',0.890196078431372,0.87843137254902,
0.831372549019608);
#2559=COLOUR_RGB('Opaque(31,36,43)',0.12156862745098,0.141176470588235,
0.168627450980392);
ENDSEC;
END-ISO-10303-21;
